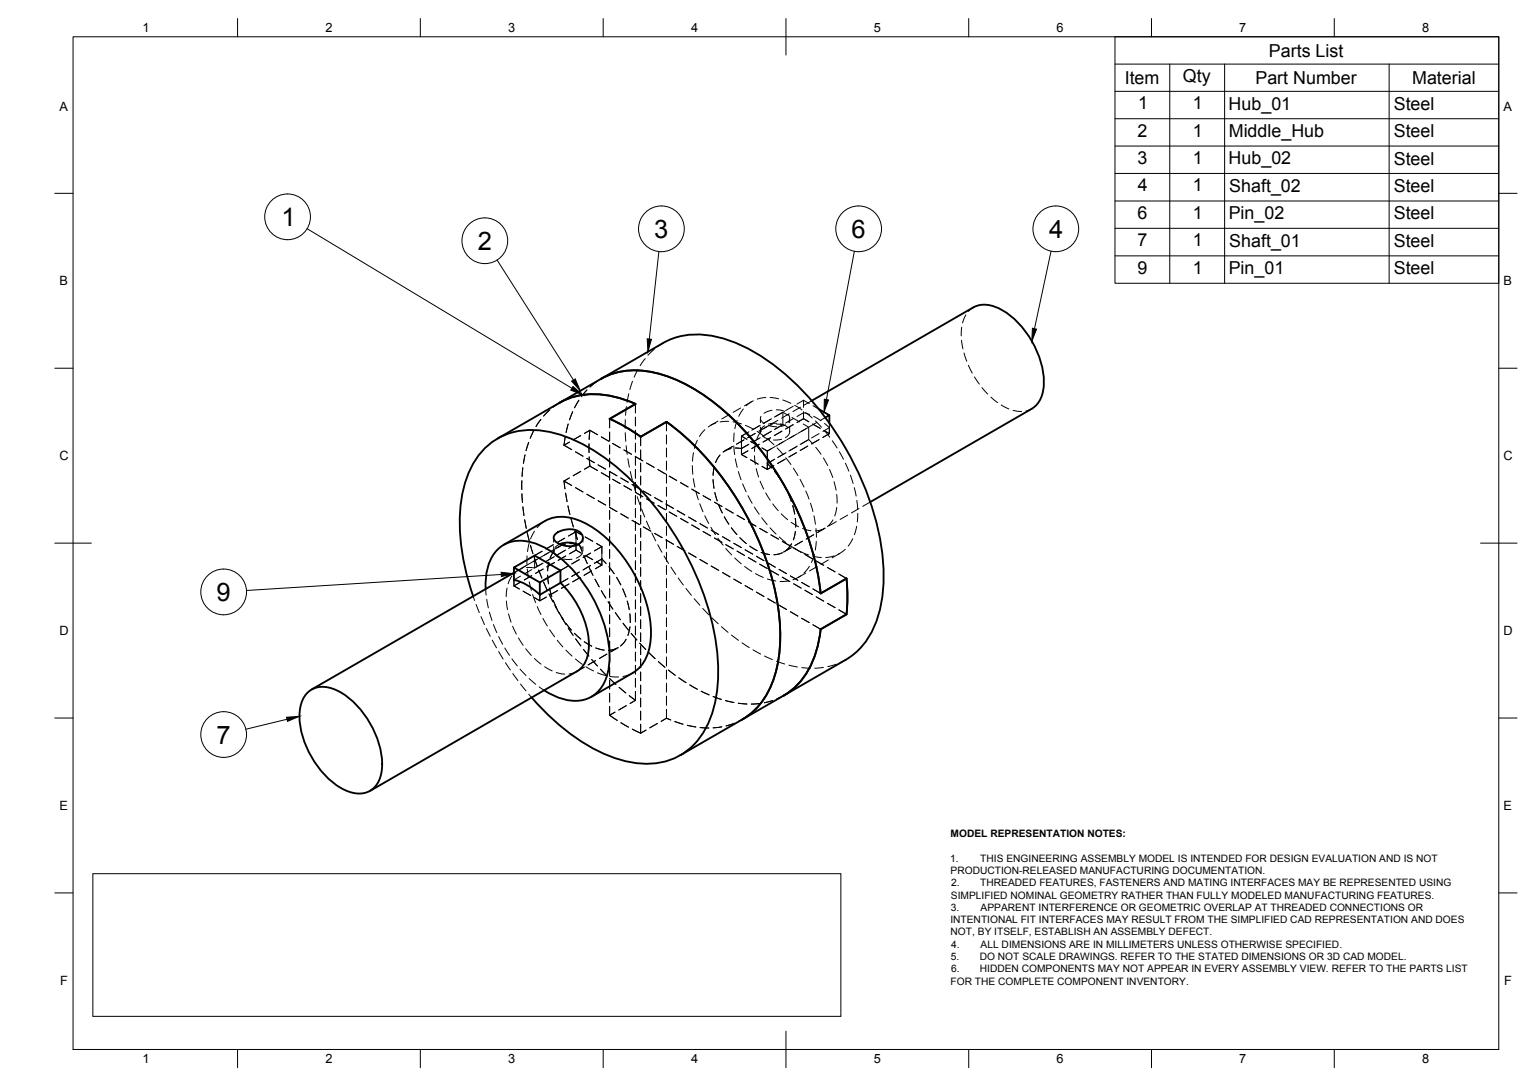
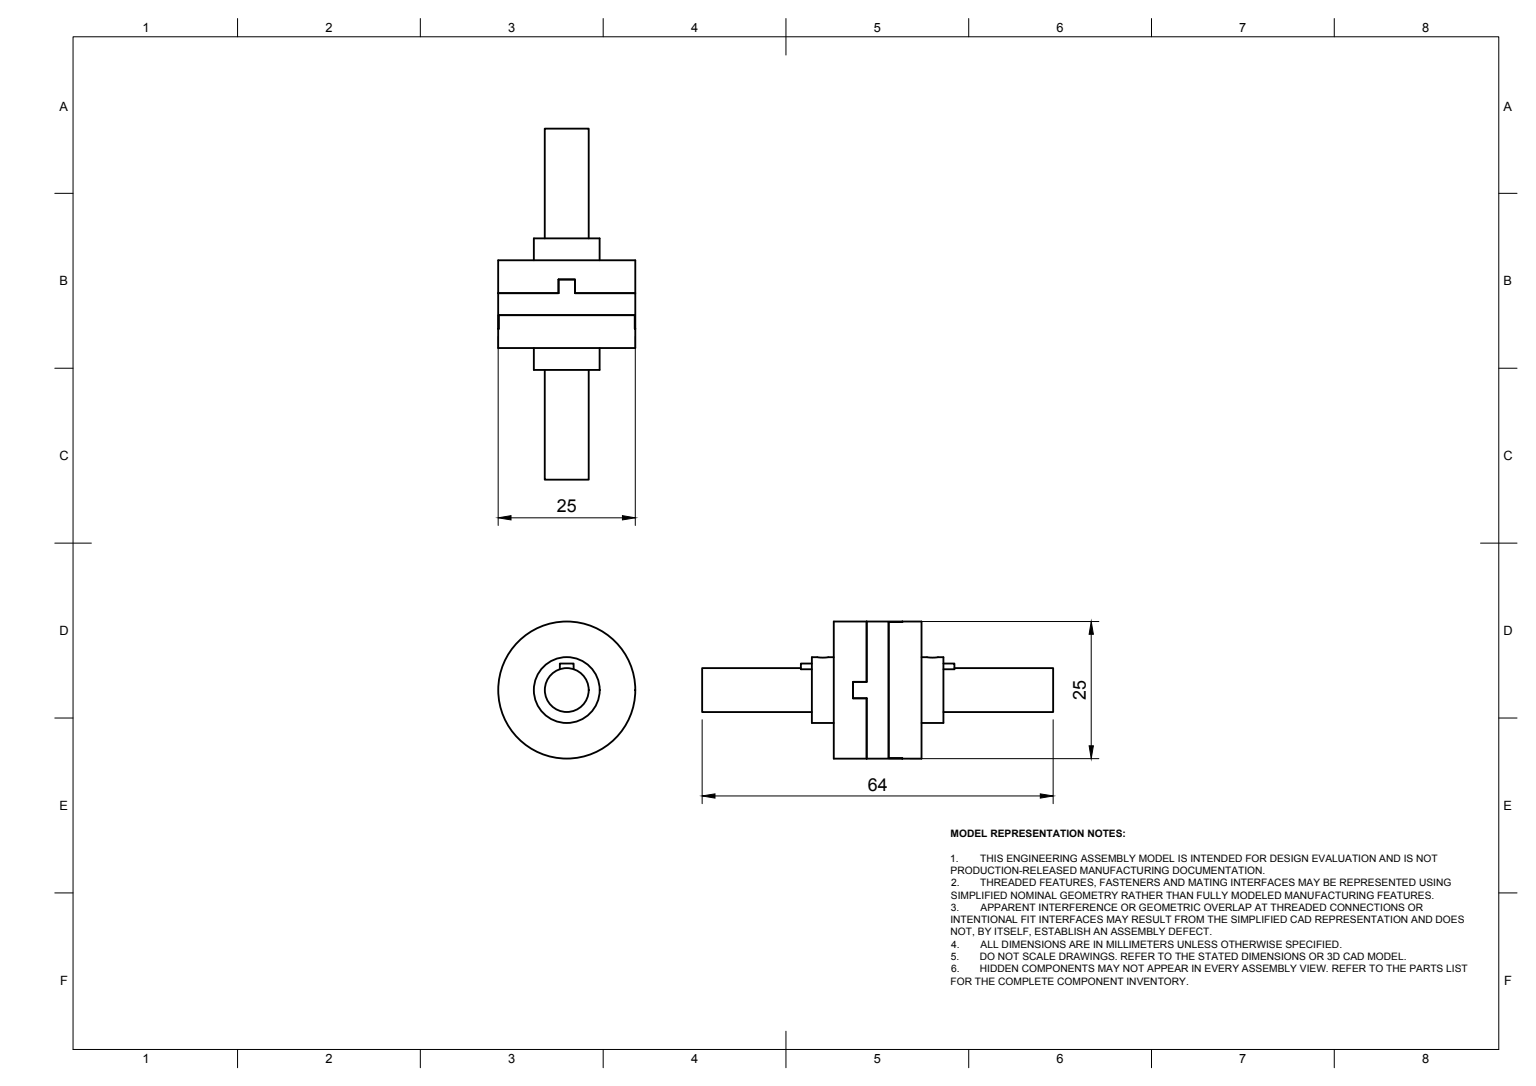
ISO-10303-21;
HEADER;
/* Generated by software containing ST-Developer
 * from STEP Tools, Inc. (www.steptools.com) 
 */

FILE_DESCRIPTION(
/* description */ (''),
/* implementation_level */ '2;1');

FILE_NAME(
/* name */ 'BR-256',
/* time_stamp */ '2026-10-05T22:24:12-07:00',
/* author */ (''),
/* organization */ (''),
/* preprocessor_version */ 'ST-DEVELOPER v20.2',
/* originating_system */ 'Autodesk Translation Framework v15.15.0.0',
/* authorisation */ '');

FILE_SCHEMA (('AUTOMOTIVE_DESIGN { 1 0 10303 214 3 1 1 }'));
ENDSEC;

DATA;
#10=MECHANICAL_DESIGN_GEOMETRIC_PRESENTATION_REPRESENTATION('',(#53,#54,
#55,#56,#57,#58,#59),#2116);
#11=ITEM_DEFINED_TRANSFORMATION($,$,#1233,#1347);
#12=ITEM_DEFINED_TRANSFORMATION($,$,#1260,#1348);
#13=ITEM_DEFINED_TRANSFORMATION($,$,#1282,#1349);
#14=ITEM_DEFINED_TRANSFORMATION($,$,#1309,#1350);
#15=ITEM_DEFINED_TRANSFORMATION($,$,#1321,#1351);
#16=ITEM_DEFINED_TRANSFORMATION($,$,#1328,#1352);
#17=ITEM_DEFINED_TRANSFORMATION($,$,#1340,#1353);
#18=(
REPRESENTATION_RELATIONSHIP($,$,#2145,#2144)
REPRESENTATION_RELATIONSHIP_WITH_TRANSFORMATION(#11)
SHAPE_REPRESENTATION_RELATIONSHIP()
);
#19=(
REPRESENTATION_RELATIONSHIP($,$,#2146,#2144)
REPRESENTATION_RELATIONSHIP_WITH_TRANSFORMATION(#12)
SHAPE_REPRESENTATION_RELATIONSHIP()
);
#20=(
REPRESENTATION_RELATIONSHIP($,$,#2147,#2144)
REPRESENTATION_RELATIONSHIP_WITH_TRANSFORMATION(#13)
SHAPE_REPRESENTATION_RELATIONSHIP()
);
#21=(
REPRESENTATION_RELATIONSHIP($,$,#2148,#2144)
REPRESENTATION_RELATIONSHIP_WITH_TRANSFORMATION(#14)
SHAPE_REPRESENTATION_RELATIONSHIP()
);
#22=(
REPRESENTATION_RELATIONSHIP($,$,#2149,#2144)
REPRESENTATION_RELATIONSHIP_WITH_TRANSFORMATION(#15)
SHAPE_REPRESENTATION_RELATIONSHIP()
);
#23=(
REPRESENTATION_RELATIONSHIP($,$,#2150,#2144)
REPRESENTATION_RELATIONSHIP_WITH_TRANSFORMATION(#16)
SHAPE_REPRESENTATION_RELATIONSHIP()
);
#24=(
REPRESENTATION_RELATIONSHIP($,$,#2151,#2144)
REPRESENTATION_RELATIONSHIP_WITH_TRANSFORMATION(#17)
SHAPE_REPRESENTATION_RELATIONSHIP()
);
#25=CONTEXT_DEPENDENT_SHAPE_REPRESENTATION(#18,#2137);
#26=CONTEXT_DEPENDENT_SHAPE_REPRESENTATION(#19,#2138);
#27=CONTEXT_DEPENDENT_SHAPE_REPRESENTATION(#20,#2139);
#28=CONTEXT_DEPENDENT_SHAPE_REPRESENTATION(#21,#2140);
#29=CONTEXT_DEPENDENT_SHAPE_REPRESENTATION(#22,#2141);
#30=CONTEXT_DEPENDENT_SHAPE_REPRESENTATION(#23,#2142);
#31=CONTEXT_DEPENDENT_SHAPE_REPRESENTATION(#24,#2143);
#32=NEXT_ASSEMBLY_USAGE_OCCURRENCE('Hub_01:1','Hub_01:1','Hub_01:1',#2153,
#2154,'Hub_01:1');
#33=NEXT_ASSEMBLY_USAGE_OCCURRENCE('Middle_Hub:1','Middle_Hub:1',
'Middle_Hub:1',#2153,#2155,'Middle_Hub:1');
#34=NEXT_ASSEMBLY_USAGE_OCCURRENCE('Hub_02:1','Hub_02:1','Hub_02:1',#2153,
#2156,'Hub_02:1');
#35=NEXT_ASSEMBLY_USAGE_OCCURRENCE('Shaft_02:1','Shaft_02:1',
'Shaft_02:1',#2153,#2157,'Shaft_02:1');
#36=NEXT_ASSEMBLY_USAGE_OCCURRENCE('Pin_02:1','Pin_02:1','Pin_02:1',#2153,
#2158,'Pin_02:1');
#37=NEXT_ASSEMBLY_USAGE_OCCURRENCE('Shaft_01:1','Shaft_01:1',
'Shaft_01:1',#2153,#2159,'Shaft_01:1');
#38=NEXT_ASSEMBLY_USAGE_OCCURRENCE('Pin_01:1','Pin_01:1','Pin_01:1',#2153,
#2160,'Pin_01:1');
#39=SHAPE_REPRESENTATION_RELATIONSHIP('SRR','None',#2145,#46);
#40=SHAPE_REPRESENTATION_RELATIONSHIP('SRR','None',#2146,#47);
#41=SHAPE_REPRESENTATION_RELATIONSHIP('SRR','None',#2147,#48);
#42=SHAPE_REPRESENTATION_RELATIONSHIP('SRR','None',#2148,#49);
#43=SHAPE_REPRESENTATION_RELATIONSHIP('SRR','None',#2149,#50);
#44=SHAPE_REPRESENTATION_RELATIONSHIP('SRR','None',#2150,#51);
#45=SHAPE_REPRESENTATION_RELATIONSHIP('SRR','None',#2151,#52);
#46=ADVANCED_BREP_SHAPE_REPRESENTATION('',(#60),#2109);
#47=ADVANCED_BREP_SHAPE_REPRESENTATION('',(#61),#2110);
#48=ADVANCED_BREP_SHAPE_REPRESENTATION('',(#62),#2111);
#49=ADVANCED_BREP_SHAPE_REPRESENTATION('',(#63),#2112);
#50=ADVANCED_BREP_SHAPE_REPRESENTATION('',(#64),#2113);
#51=ADVANCED_BREP_SHAPE_REPRESENTATION('',(#65),#2114);
#52=ADVANCED_BREP_SHAPE_REPRESENTATION('',(#66),#2115);
#53=STYLED_ITEM('',(#2189),#60);
#54=STYLED_ITEM('',(#2190),#61);
#55=STYLED_ITEM('',(#2191),#62);
#56=STYLED_ITEM('',(#2192),#63);
#57=STYLED_ITEM('',(#2192),#64);
#58=STYLED_ITEM('',(#2192),#65);
#59=STYLED_ITEM('',(#2192),#66);
#60=MANIFOLD_SOLID_BREP('Body1',#1147);
#61=MANIFOLD_SOLID_BREP('Body1',#1148);
#62=MANIFOLD_SOLID_BREP('Body1',#1149);
#63=MANIFOLD_SOLID_BREP('Body1',#1150);
#64=MANIFOLD_SOLID_BREP('Body1',#1151);
#65=MANIFOLD_SOLID_BREP('Body1',#1152);
#66=MANIFOLD_SOLID_BREP('Body1',#1153);
#67=FACE_BOUND('',#201,.T.);
#68=FACE_BOUND('',#211,.T.);
#69=FACE_BOUND('',#213,.T.);
#70=FACE_BOUND('',#215,.T.);
#71=FACE_BOUND('',#230,.T.);
#72=FACE_BOUND('',#234,.T.);
#73=FACE_BOUND('',#237,.T.);
#74=FACE_BOUND('',#239,.T.);
#75=PLANE('',#1236);
#76=PLANE('',#1237);
#77=PLANE('',#1238);
#78=PLANE('',#1239);
#79=PLANE('',#1243);
#80=PLANE('',#1244);
#81=PLANE('',#1245);
#82=PLANE('',#1248);
#83=PLANE('',#1250);
#84=PLANE('',#1256);
#85=PLANE('',#1257);
#86=PLANE('',#1261);
#87=PLANE('',#1262);
#88=PLANE('',#1263);
#89=PLANE('',#1267);
#90=PLANE('',#1269);
#91=PLANE('',#1271);
#92=PLANE('',#1272);
#93=PLANE('',#1273);
#94=PLANE('',#1276);
#95=PLANE('',#1278);
#96=PLANE('',#1285);
#97=PLANE('',#1286);
#98=PLANE('',#1287);
#99=PLANE('',#1288);
#100=PLANE('',#1295);
#101=PLANE('',#1297);
#102=PLANE('',#1298);
#103=PLANE('',#1299);
#104=PLANE('',#1303);
#105=PLANE('',#1305);
#106=PLANE('',#1308);
#107=PLANE('',#1310);
#108=PLANE('',#1311);
#109=PLANE('',#1312);
#110=PLANE('',#1313);
#111=PLANE('',#1315);
#112=PLANE('',#1320);
#113=PLANE('',#1322);
#114=PLANE('',#1323);
#115=PLANE('',#1324);
#116=PLANE('',#1325);
#117=PLANE('',#1326);
#118=PLANE('',#1327);
#119=PLANE('',#1329);
#120=PLANE('',#1330);
#121=PLANE('',#1332);
#122=PLANE('',#1333);
#123=PLANE('',#1338);
#124=PLANE('',#1339);
#125=PLANE('',#1341);
#126=PLANE('',#1342);
#127=PLANE('',#1343);
#128=PLANE('',#1344);
#129=PLANE('',#1345);
#130=PLANE('',#1346);
#131=FACE_OUTER_BOUND('',#198,.T.);
#132=FACE_OUTER_BOUND('',#199,.T.);
#133=FACE_OUTER_BOUND('',#200,.T.);
#134=FACE_OUTER_BOUND('',#202,.T.);
#135=FACE_OUTER_BOUND('',#203,.T.);
#136=FACE_OUTER_BOUND('',#204,.T.);
#137=FACE_OUTER_BOUND('',#205,.T.);
#138=FACE_OUTER_BOUND('',#206,.T.);
#139=FACE_OUTER_BOUND('',#207,.T.);
#140=FACE_OUTER_BOUND('',#208,.T.);
#141=FACE_OUTER_BOUND('',#209,.T.);
#142=FACE_OUTER_BOUND('',#210,.T.);
#143=FACE_OUTER_BOUND('',#212,.T.);
#144=FACE_OUTER_BOUND('',#214,.T.);
#145=FACE_OUTER_BOUND('',#216,.T.);
#146=FACE_OUTER_BOUND('',#217,.T.);
#147=FACE_OUTER_BOUND('',#218,.T.);
#148=FACE_OUTER_BOUND('',#219,.T.);
#149=FACE_OUTER_BOUND('',#220,.T.);
#150=FACE_OUTER_BOUND('',#221,.T.);
#151=FACE_OUTER_BOUND('',#222,.T.);
#152=FACE_OUTER_BOUND('',#223,.T.);
#153=FACE_OUTER_BOUND('',#224,.T.);
#154=FACE_OUTER_BOUND('',#225,.T.);
#155=FACE_OUTER_BOUND('',#226,.T.);
#156=FACE_OUTER_BOUND('',#227,.T.);
#157=FACE_OUTER_BOUND('',#228,.T.);
#158=FACE_OUTER_BOUND('',#229,.T.);
#159=FACE_OUTER_BOUND('',#231,.T.);
#160=FACE_OUTER_BOUND('',#232,.T.);
#161=FACE_OUTER_BOUND('',#233,.T.);
#162=FACE_OUTER_BOUND('',#235,.T.);
#163=FACE_OUTER_BOUND('',#236,.T.);
#164=FACE_OUTER_BOUND('',#238,.T.);
#165=FACE_OUTER_BOUND('',#240,.T.);
#166=FACE_OUTER_BOUND('',#241,.T.);
#167=FACE_OUTER_BOUND('',#242,.T.);
#168=FACE_OUTER_BOUND('',#243,.T.);
#169=FACE_OUTER_BOUND('',#244,.T.);
#170=FACE_OUTER_BOUND('',#245,.T.);
#171=FACE_OUTER_BOUND('',#246,.T.);
#172=FACE_OUTER_BOUND('',#247,.T.);
#173=FACE_OUTER_BOUND('',#248,.T.);
#174=FACE_OUTER_BOUND('',#249,.T.);
#175=FACE_OUTER_BOUND('',#250,.T.);
#176=FACE_OUTER_BOUND('',#251,.T.);
#177=FACE_OUTER_BOUND('',#252,.T.);
#178=FACE_OUTER_BOUND('',#253,.T.);
#179=FACE_OUTER_BOUND('',#254,.T.);
#180=FACE_OUTER_BOUND('',#255,.T.);
#181=FACE_OUTER_BOUND('',#256,.T.);
#182=FACE_OUTER_BOUND('',#257,.T.);
#183=FACE_OUTER_BOUND('',#258,.T.);
#184=FACE_OUTER_BOUND('',#259,.T.);
#185=FACE_OUTER_BOUND('',#260,.T.);
#186=FACE_OUTER_BOUND('',#261,.T.);
#187=FACE_OUTER_BOUND('',#262,.T.);
#188=FACE_OUTER_BOUND('',#263,.T.);
#189=FACE_OUTER_BOUND('',#264,.T.);
#190=FACE_OUTER_BOUND('',#265,.T.);
#191=FACE_OUTER_BOUND('',#266,.T.);
#192=FACE_OUTER_BOUND('',#267,.T.);
#193=FACE_OUTER_BOUND('',#268,.T.);
#194=FACE_OUTER_BOUND('',#269,.T.);
#195=FACE_OUTER_BOUND('',#270,.T.);
#196=FACE_OUTER_BOUND('',#271,.T.);
#197=FACE_OUTER_BOUND('',#272,.T.);
#198=EDGE_LOOP('',(#773,#774,#775,#776));
#199=EDGE_LOOP('',(#777,#778,#779,#780));
#200=EDGE_LOOP('',(#781,#782,#783,#784));
#201=EDGE_LOOP('',(#785));
#202=EDGE_LOOP('',(#786,#787,#788,#789));
#203=EDGE_LOOP('',(#790,#791,#792,#793));
#204=EDGE_LOOP('',(#794,#795,#796,#797));
#205=EDGE_LOOP('',(#798,#799,#800,#801));
#206=EDGE_LOOP('',(#802,#803,#804,#805));
#207=EDGE_LOOP('',(#806,#807,#808,#809));
#208=EDGE_LOOP('',(#810,#811));
#209=EDGE_LOOP('',(#812,#813,#814));
#210=EDGE_LOOP('',(#815,#816,#817,#818));
#211=EDGE_LOOP('',(#819));
#212=EDGE_LOOP('',(#820));
#213=EDGE_LOOP('',(#821,#822,#823,#824));
#214=EDGE_LOOP('',(#825));
#215=EDGE_LOOP('',(#826));
#216=EDGE_LOOP('',(#827,#828,#829,#830,#831,#832,#833,#834,#835,#836,#837,
#838));
#217=EDGE_LOOP('',(#839,#840,#841,#842));
#218=EDGE_LOOP('',(#843,#844,#845,#846));
#219=EDGE_LOOP('',(#847,#848,#849,#850,#851));
#220=EDGE_LOOP('',(#852,#853));
#221=EDGE_LOOP('',(#854,#855));
#222=EDGE_LOOP('',(#856,#857,#858,#859));
#223=EDGE_LOOP('',(#860,#861,#862,#863));
#224=EDGE_LOOP('',(#864,#865,#866,#867));
#225=EDGE_LOOP('',(#868,#869));
#226=EDGE_LOOP('',(#870,#871,#872));
#227=EDGE_LOOP('',(#873,#874,#875,#876,#877,#878,#879,#880,#881,#882,#883,
#884,#885,#886,#887,#888,#889,#890,#891,#892));
#228=EDGE_LOOP('',(#893,#894,#895,#896,#897));
#229=EDGE_LOOP('',(#898,#899,#900,#901));
#230=EDGE_LOOP('',(#902));
#231=EDGE_LOOP('',(#903,#904,#905,#906));
#232=EDGE_LOOP('',(#907,#908,#909,#910));
#233=EDGE_LOOP('',(#911));
#234=EDGE_LOOP('',(#912,#913,#914,#915));
#235=EDGE_LOOP('',(#916,#917,#918,#919));
#236=EDGE_LOOP('',(#920,#921,#922,#923));
#237=EDGE_LOOP('',(#924,#925));
#238=EDGE_LOOP('',(#926));
#239=EDGE_LOOP('',(#927));
#240=EDGE_LOOP('',(#928,#929,#930,#931));
#241=EDGE_LOOP('',(#932,#933,#934,#935));
#242=EDGE_LOOP('',(#936,#937,#938,#939,#940));
#243=EDGE_LOOP('',(#941,#942));
#244=EDGE_LOOP('',(#943,#944));
#245=EDGE_LOOP('',(#945,#946,#947,#948,#949,#950,#951,#952,#953,#954,#955,
#956));
#246=EDGE_LOOP('',(#957,#958,#959,#960));
#247=EDGE_LOOP('',(#961,#962,#963,#964));
#248=EDGE_LOOP('',(#965,#966,#967,#968));
#249=EDGE_LOOP('',(#969,#970,#971,#972));
#250=EDGE_LOOP('',(#973,#974,#975,#976));
#251=EDGE_LOOP('',(#977,#978,#979,#980,#981));
#252=EDGE_LOOP('',(#982,#983,#984,#985,#986,#987,#988,#989));
#253=EDGE_LOOP('',(#990));
#254=EDGE_LOOP('',(#991,#992,#993,#994));
#255=EDGE_LOOP('',(#995,#996,#997,#998));
#256=EDGE_LOOP('',(#999,#1000,#1001,#1002));
#257=EDGE_LOOP('',(#1003,#1004,#1005,#1006));
#258=EDGE_LOOP('',(#1007,#1008,#1009,#1010));
#259=EDGE_LOOP('',(#1011,#1012,#1013,#1014));
#260=EDGE_LOOP('',(#1015,#1016,#1017,#1018));
#261=EDGE_LOOP('',(#1019,#1020,#1021,#1022));
#262=EDGE_LOOP('',(#1023,#1024,#1025,#1026));
#263=EDGE_LOOP('',(#1027,#1028,#1029,#1030));
#264=EDGE_LOOP('',(#1031,#1032,#1033,#1034,#1035,#1036,#1037,#1038));
#265=EDGE_LOOP('',(#1039));
#266=EDGE_LOOP('',(#1040,#1041,#1042,#1043,#1044));
#267=EDGE_LOOP('',(#1045,#1046,#1047,#1048));
#268=EDGE_LOOP('',(#1049,#1050,#1051,#1052));
#269=EDGE_LOOP('',(#1053,#1054,#1055,#1056));
#270=EDGE_LOOP('',(#1057,#1058,#1059,#1060));
#271=EDGE_LOOP('',(#1061,#1062,#1063,#1064));
#272=EDGE_LOOP('',(#1065,#1066,#1067,#1068));
#273=B_SPLINE_CURVE_WITH_KNOTS('',3,(#1710,#1711,#1712,#1713,#1714,#1715,
#1716,#1717,#1718,#1719,#1720,#1721,#1722,#1723,#1724,#1725,#1726,#1727,
#1728,#1729,#1730,#1731,#1732,#1733,#1734,#1735,#1736,#1737,#1738,#1739,
#1740,#1741,#1742,#1743),.UNSPECIFIED.,.T.,.F.,(4,2,2,2,2,2,2,2,2,2,2,2,
2,2,2,2,4),(0.,0.0377449625945589,0.0754899251891177,0.113233879657539,
0.150977834125959,0.18872178859438,0.226465743062801,0.26421070565736,0.301955668251919,
0.339700630846477,0.377445593441036,0.415189547909457,0.452933502377878,
0.490677456846299,0.52842141131472,0.566166373909278,0.603911336503837),
 .UNSPECIFIED.);
#274=B_SPLINE_CURVE_WITH_KNOTS('',3,(#1872,#1873,#1874,#1875,#1876,#1877,
#1878,#1879,#1880,#1881,#1882,#1883,#1884,#1885,#1886,#1887,#1888,#1889),
 .UNSPECIFIED.,.F.,.F.,(4,2,2,2,2,2,2,2,4),(0.,0.0377449625945587,0.0754899251891175,
0.113233879657538,0.150977834125959,0.18872178859438,0.226465743062801,
0.264210705657359,0.301955668251918),.UNSPECIFIED.);
#275=B_SPLINE_CURVE_WITH_KNOTS('',3,(#1890,#1891,#1892,#1893,#1894,#1895,
#1896,#1897,#1898,#1899,#1900,#1901,#1902,#1903,#1904,#1905,#1906,#1907),
 .UNSPECIFIED.,.F.,.F.,(4,2,2,2,2,2,2,2,4),(0.301955668251918,0.339700630846477,
0.377445593441036,0.415189547909457,0.452933502377877,0.490677456846298,
0.528421411314719,0.566166373909278,0.603911336503836),.UNSPECIFIED.);
#276=LINE('',#1709,#381);
#277=LINE('',#1747,#382);
#278=LINE('',#1749,#383);
#279=LINE('',#1751,#384);
#280=LINE('',#1752,#385);
#281=LINE('',#1755,#386);
#282=LINE('',#1757,#387);
#283=LINE('',#1758,#388);
#284=LINE('',#1761,#389);
#285=LINE('',#1763,#390);
#286=LINE('',#1764,#391);
#287=LINE('',#1772,#392);
#288=LINE('',#1774,#393);
#289=LINE('',#1776,#394);
#290=LINE('',#1777,#395);
#291=LINE('',#1781,#396);
#292=LINE('',#1783,#397);
#293=LINE('',#1785,#398);
#294=LINE('',#1786,#399);
#295=LINE('',#1800,#400);
#296=LINE('',#1807,#401);
#297=LINE('',#1812,#402);
#298=LINE('',#1814,#403);
#299=LINE('',#1816,#404);
#300=LINE('',#1817,#405);
#301=LINE('',#1821,#406);
#302=LINE('',#1823,#407);
#303=LINE('',#1825,#408);
#304=LINE('',#1826,#409);
#305=LINE('',#1839,#410);
#306=LINE('',#1841,#411);
#307=LINE('',#1843,#412);
#308=LINE('',#1844,#413);
#309=LINE('',#1848,#414);
#310=LINE('',#1850,#415);
#311=LINE('',#1852,#416);
#312=LINE('',#1853,#417);
#313=LINE('',#1864,#418);
#314=LINE('',#1870,#419);
#315=LINE('',#1911,#420);
#316=LINE('',#1913,#421);
#317=LINE('',#1915,#422);
#318=LINE('',#1916,#423);
#319=LINE('',#1919,#424);
#320=LINE('',#1921,#425);
#321=LINE('',#1922,#426);
#322=LINE('',#1925,#427);
#323=LINE('',#1927,#428);
#324=LINE('',#1928,#429);
#325=LINE('',#1937,#430);
#326=LINE('',#1945,#431);
#327=LINE('',#1947,#432);
#328=LINE('',#1949,#433);
#329=LINE('',#1950,#434);
#330=LINE('',#1954,#435);
#331=LINE('',#1956,#436);
#332=LINE('',#1958,#437);
#333=LINE('',#1959,#438);
#334=LINE('',#1970,#439);
#335=LINE('',#1976,#440);
#336=LINE('',#1978,#441);
#337=LINE('',#1980,#442);
#338=LINE('',#1981,#443);
#339=LINE('',#1984,#444);
#340=LINE('',#1986,#445);
#341=LINE('',#1987,#446);
#342=LINE('',#1991,#447);
#343=LINE('',#1992,#448);
#344=LINE('',#1993,#449);
#345=LINE('',#2002,#450);
#346=LINE('',#2009,#451);
#347=LINE('',#2011,#452);
#348=LINE('',#2013,#453);
#349=LINE('',#2014,#454);
#350=LINE('',#2017,#455);
#351=LINE('',#2019,#456);
#352=LINE('',#2020,#457);
#353=LINE('',#2023,#458);
#354=LINE('',#2025,#459);
#355=LINE('',#2026,#460);
#356=LINE('',#2028,#461);
#357=LINE('',#2029,#462);
#358=LINE('',#2036,#463);
#359=LINE('',#2038,#464);
#360=LINE('',#2040,#465);
#361=LINE('',#2041,#466);
#362=LINE('',#2046,#467);
#363=LINE('',#2047,#468);
#364=LINE('',#2050,#469);
#365=LINE('',#2051,#470);
#366=LINE('',#2054,#471);
#367=LINE('',#2055,#472);
#368=LINE('',#2060,#473);
#369=LINE('',#2069,#474);
#370=LINE('',#2071,#475);
#371=LINE('',#2073,#476);
#372=LINE('',#2074,#477);
#373=LINE('',#2077,#478);
#374=LINE('',#2079,#479);
#375=LINE('',#2080,#480);
#376=LINE('',#2083,#481);
#377=LINE('',#2085,#482);
#378=LINE('',#2086,#483);
#379=LINE('',#2088,#484);
#380=LINE('',#2089,#485);
#381=VECTOR('',#1362,1.);
#382=VECTOR('',#1365,10.);
#383=VECTOR('',#1366,10.);
#384=VECTOR('',#1367,10.);
#385=VECTOR('',#1368,10.);
#386=VECTOR('',#1371,10.);
#387=VECTOR('',#1372,10.);
#388=VECTOR('',#1373,10.);
#389=VECTOR('',#1376,10.);
#390=VECTOR('',#1377,10.);
#391=VECTOR('',#1378,10.);
#392=VECTOR('',#1389,10.);
#393=VECTOR('',#1390,10.);
#394=VECTOR('',#1391,10.);
#395=VECTOR('',#1392,10.);
#396=VECTOR('',#1395,10.);
#397=VECTOR('',#1396,10.);
#398=VECTOR('',#1397,10.);
#399=VECTOR('',#1398,10.);
#400=VECTOR('',#1419,6.);
#401=VECTOR('',#1430,12.5);
#402=VECTOR('',#1435,10.);
#403=VECTOR('',#1436,10.);
#404=VECTOR('',#1437,10.);
#405=VECTOR('',#1438,10.);
#406=VECTOR('',#1441,10.);
#407=VECTOR('',#1442,10.);
#408=VECTOR('',#1443,10.);
#409=VECTOR('',#1444,10.);
#410=VECTOR('',#1463,10.);
#411=VECTOR('',#1464,10.);
#412=VECTOR('',#1465,10.);
#413=VECTOR('',#1466,10.);
#414=VECTOR('',#1469,10.);
#415=VECTOR('',#1470,10.);
#416=VECTOR('',#1471,10.);
#417=VECTOR('',#1472,10.);
#418=VECTOR('',#1491,12.5);
#419=VECTOR('',#1498,0.999999999999999);
#420=VECTOR('',#1501,10.);
#421=VECTOR('',#1502,10.);
#422=VECTOR('',#1503,10.);
#423=VECTOR('',#1504,10.);
#424=VECTOR('',#1507,10.);
#425=VECTOR('',#1508,10.);
#426=VECTOR('',#1509,10.);
#427=VECTOR('',#1512,10.);
#428=VECTOR('',#1513,10.);
#429=VECTOR('',#1514,10.);
#430=VECTOR('',#1527,6.);
#431=VECTOR('',#1536,10.);
#432=VECTOR('',#1537,10.);
#433=VECTOR('',#1538,10.);
#434=VECTOR('',#1539,10.);
#435=VECTOR('',#1542,10.);
#436=VECTOR('',#1543,10.);
#437=VECTOR('',#1544,10.);
#438=VECTOR('',#1545,10.);
#439=VECTOR('',#1564,12.5);
#440=VECTOR('',#1571,10.);
#441=VECTOR('',#1572,10.);
#442=VECTOR('',#1573,10.);
#443=VECTOR('',#1574,10.);
#444=VECTOR('',#1577,10.);
#445=VECTOR('',#1578,10.);
#446=VECTOR('',#1579,10.);
#447=VECTOR('',#1582,10.);
#448=VECTOR('',#1583,10.);
#449=VECTOR('',#1584,10.);
#450=VECTOR('',#1597,4.);
#451=VECTOR('',#1606,10.);
#452=VECTOR('',#1607,10.);
#453=VECTOR('',#1608,10.);
#454=VECTOR('',#1609,10.);
#455=VECTOR('',#1612,10.);
#456=VECTOR('',#1613,10.);
#457=VECTOR('',#1614,10.);
#458=VECTOR('',#1617,10.);
#459=VECTOR('',#1618,10.);
#460=VECTOR('',#1619,10.);
#461=VECTOR('',#1622,10.);
#462=VECTOR('',#1623,10.);
#463=VECTOR('',#1632,10.);
#464=VECTOR('',#1633,10.);
#465=VECTOR('',#1634,10.);
#466=VECTOR('',#1635,10.);
#467=VECTOR('',#1640,10.);
#468=VECTOR('',#1641,10.);
#469=VECTOR('',#1644,10.);
#470=VECTOR('',#1645,10.);
#471=VECTOR('',#1648,10.);
#472=VECTOR('',#1649,10.);
#473=VECTOR('',#1654,4.);
#474=VECTOR('',#1667,10.);
#475=VECTOR('',#1668,10.);
#476=VECTOR('',#1669,10.);
#477=VECTOR('',#1670,10.);
#478=VECTOR('',#1673,10.);
#479=VECTOR('',#1674,10.);
#480=VECTOR('',#1675,10.);
#481=VECTOR('',#1678,10.);
#482=VECTOR('',#1679,10.);
#483=VECTOR('',#1680,10.);
#484=VECTOR('',#1683,10.);
#485=VECTOR('',#1684,10.);
#486=CIRCLE('',#1235,1.);
#487=CIRCLE('',#1240,4.);
#488=CIRCLE('',#1242,4.);
#489=CIRCLE('',#1246,12.5);
#490=CIRCLE('',#1247,12.5);
#491=CIRCLE('',#1249,12.5);
#492=CIRCLE('',#1251,12.5);
#493=CIRCLE('',#1252,12.5);
#494=CIRCLE('',#1254,6.);
#495=CIRCLE('',#1255,6.);
#496=CIRCLE('',#1258,12.5);
#497=CIRCLE('',#1264,12.5);
#498=CIRCLE('',#1265,12.5);
#499=CIRCLE('',#1266,12.5);
#500=CIRCLE('',#1268,12.5);
#501=CIRCLE('',#1270,12.5);
#502=CIRCLE('',#1274,12.5);
#503=CIRCLE('',#1275,12.5);
#504=CIRCLE('',#1277,12.5);
#505=CIRCLE('',#1279,12.5);
#506=CIRCLE('',#1280,12.5);
#507=CIRCLE('',#1284,0.999999999999999);
#508=CIRCLE('',#1289,6.);
#509=CIRCLE('',#1290,4.);
#510=CIRCLE('',#1292,4.);
#511=CIRCLE('',#1294,6.);
#512=CIRCLE('',#1296,12.5);
#513=CIRCLE('',#1300,12.5);
#514=CIRCLE('',#1301,12.5);
#515=CIRCLE('',#1302,12.5);
#516=CIRCLE('',#1304,12.5);
#517=CIRCLE('',#1306,12.5);
#518=CIRCLE('',#1314,4.);
#519=CIRCLE('',#1316,4.);
#520=CIRCLE('',#1317,4.);
#521=CIRCLE('',#1319,4.);
#522=CIRCLE('',#1331,4.);
#523=CIRCLE('',#1335,4.);
#524=CIRCLE('',#1336,4.);
#525=CIRCLE('',#1337,4.);
#526=VERTEX_POINT('',#1706);
#527=VERTEX_POINT('',#1708);
#528=VERTEX_POINT('',#1745);
#529=VERTEX_POINT('',#1746);
#530=VERTEX_POINT('',#1748);
#531=VERTEX_POINT('',#1750);
#532=VERTEX_POINT('',#1754);
#533=VERTEX_POINT('',#1756);
#534=VERTEX_POINT('',#1760);
#535=VERTEX_POINT('',#1762);
#536=VERTEX_POINT('',#1770);
#537=VERTEX_POINT('',#1771);
#538=VERTEX_POINT('',#1773);
#539=VERTEX_POINT('',#1775);
#540=VERTEX_POINT('',#1779);
#541=VERTEX_POINT('',#1780);
#542=VERTEX_POINT('',#1782);
#543=VERTEX_POINT('',#1784);
#544=VERTEX_POINT('',#1793);
#545=VERTEX_POINT('',#1797);
#546=VERTEX_POINT('',#1799);
#547=VERTEX_POINT('',#1804);
#548=VERTEX_POINT('',#1810);
#549=VERTEX_POINT('',#1811);
#550=VERTEX_POINT('',#1813);
#551=VERTEX_POINT('',#1815);
#552=VERTEX_POINT('',#1819);
#553=VERTEX_POINT('',#1820);
#554=VERTEX_POINT('',#1822);
#555=VERTEX_POINT('',#1824);
#556=VERTEX_POINT('',#1829);
#557=VERTEX_POINT('',#1837);
#558=VERTEX_POINT('',#1838);
#559=VERTEX_POINT('',#1840);
#560=VERTEX_POINT('',#1842);
#561=VERTEX_POINT('',#1846);
#562=VERTEX_POINT('',#1847);
#563=VERTEX_POINT('',#1849);
#564=VERTEX_POINT('',#1851);
#565=VERTEX_POINT('',#1860);
#566=VERTEX_POINT('',#1867);
#567=VERTEX_POINT('',#1869);
#568=VERTEX_POINT('',#1871);
#569=VERTEX_POINT('',#1909);
#570=VERTEX_POINT('',#1910);
#571=VERTEX_POINT('',#1912);
#572=VERTEX_POINT('',#1914);
#573=VERTEX_POINT('',#1918);
#574=VERTEX_POINT('',#1920);
#575=VERTEX_POINT('',#1924);
#576=VERTEX_POINT('',#1926);
#577=VERTEX_POINT('',#1930);
#578=VERTEX_POINT('',#1936);
#579=VERTEX_POINT('',#1940);
#580=VERTEX_POINT('',#1943);
#581=VERTEX_POINT('',#1944);
#582=VERTEX_POINT('',#1946);
#583=VERTEX_POINT('',#1948);
#584=VERTEX_POINT('',#1952);
#585=VERTEX_POINT('',#1953);
#586=VERTEX_POINT('',#1955);
#587=VERTEX_POINT('',#1957);
#588=VERTEX_POINT('',#1962);
#589=VERTEX_POINT('',#1974);
#590=VERTEX_POINT('',#1975);
#591=VERTEX_POINT('',#1977);
#592=VERTEX_POINT('',#1979);
#593=VERTEX_POINT('',#1983);
#594=VERTEX_POINT('',#1985);
#595=VERTEX_POINT('',#1989);
#596=VERTEX_POINT('',#1990);
#597=VERTEX_POINT('',#1997);
#598=VERTEX_POINT('',#2001);
#599=VERTEX_POINT('',#2007);
#600=VERTEX_POINT('',#2008);
#601=VERTEX_POINT('',#2010);
#602=VERTEX_POINT('',#2012);
#603=VERTEX_POINT('',#2016);
#604=VERTEX_POINT('',#2018);
#605=VERTEX_POINT('',#2022);
#606=VERTEX_POINT('',#2024);
#607=VERTEX_POINT('',#2034);
#608=VERTEX_POINT('',#2035);
#609=VERTEX_POINT('',#2037);
#610=VERTEX_POINT('',#2039);
#611=VERTEX_POINT('',#2043);
#612=VERTEX_POINT('',#2045);
#613=VERTEX_POINT('',#2049);
#614=VERTEX_POINT('',#2053);
#615=VERTEX_POINT('',#2057);
#616=VERTEX_POINT('',#2059);
#617=VERTEX_POINT('',#2067);
#618=VERTEX_POINT('',#2068);
#619=VERTEX_POINT('',#2070);
#620=VERTEX_POINT('',#2072);
#621=VERTEX_POINT('',#2076);
#622=VERTEX_POINT('',#2078);
#623=VERTEX_POINT('',#2082);
#624=VERTEX_POINT('',#2084);
#625=EDGE_CURVE('',#526,#526,#486,.T.);
#626=EDGE_CURVE('',#526,#527,#276,.T.);
#627=EDGE_CURVE('',#527,#527,#273,.T.);
#628=EDGE_CURVE('',#528,#529,#277,.T.);
#629=EDGE_CURVE('',#530,#528,#278,.T.);
#630=EDGE_CURVE('',#530,#531,#279,.T.);
#631=EDGE_CURVE('',#529,#531,#280,.T.);
#632=EDGE_CURVE('',#532,#528,#281,.T.);
#633=EDGE_CURVE('',#533,#532,#282,.T.);
#634=EDGE_CURVE('',#533,#530,#283,.T.);
#635=EDGE_CURVE('',#534,#532,#284,.T.);
#636=EDGE_CURVE('',#535,#534,#285,.T.);
#637=EDGE_CURVE('',#533,#535,#286,.T.);
#638=EDGE_CURVE('',#535,#531,#487,.T.);
#639=EDGE_CURVE('',#529,#534,#488,.T.);
#640=EDGE_CURVE('',#536,#537,#287,.T.);
#641=EDGE_CURVE('',#538,#536,#288,.T.);
#642=EDGE_CURVE('',#538,#539,#289,.T.);
#643=EDGE_CURVE('',#537,#539,#290,.T.);
#644=EDGE_CURVE('',#540,#541,#291,.T.);
#645=EDGE_CURVE('',#542,#540,#292,.T.);
#646=EDGE_CURVE('',#542,#543,#293,.T.);
#647=EDGE_CURVE('',#541,#543,#294,.T.);
#648=EDGE_CURVE('',#539,#542,#489,.T.);
#649=EDGE_CURVE('',#543,#538,#490,.T.);
#650=EDGE_CURVE('',#541,#540,#491,.T.);
#651=EDGE_CURVE('',#537,#544,#492,.T.);
#652=EDGE_CURVE('',#544,#536,#493,.T.);
#653=EDGE_CURVE('',#545,#545,#494,.T.);
#654=EDGE_CURVE('',#545,#546,#295,.T.);
#655=EDGE_CURVE('',#546,#546,#495,.T.);
#656=EDGE_CURVE('',#547,#547,#496,.T.);
#657=EDGE_CURVE('',#547,#544,#296,.T.);
#658=EDGE_CURVE('',#548,#549,#297,.T.);
#659=EDGE_CURVE('',#548,#550,#298,.T.);
#660=EDGE_CURVE('',#551,#550,#299,.T.);
#661=EDGE_CURVE('',#549,#551,#300,.T.);
#662=EDGE_CURVE('',#552,#553,#301,.T.);
#663=EDGE_CURVE('',#552,#554,#302,.T.);
#664=EDGE_CURVE('',#555,#554,#303,.T.);
#665=EDGE_CURVE('',#553,#555,#304,.T.);
#666=EDGE_CURVE('',#550,#555,#497,.T.);
#667=EDGE_CURVE('',#554,#556,#498,.T.);
#668=EDGE_CURVE('',#556,#551,#499,.T.);
#669=EDGE_CURVE('',#549,#548,#500,.T.);
#670=EDGE_CURVE('',#553,#552,#501,.T.);
#671=EDGE_CURVE('',#557,#558,#305,.T.);
#672=EDGE_CURVE('',#557,#559,#306,.T.);
#673=EDGE_CURVE('',#560,#559,#307,.T.);
#674=EDGE_CURVE('',#558,#560,#308,.T.);
#675=EDGE_CURVE('',#561,#562,#309,.T.);
#676=EDGE_CURVE('',#561,#563,#310,.T.);
#677=EDGE_CURVE('',#564,#563,#311,.T.);
#678=EDGE_CURVE('',#562,#564,#312,.T.);
#679=EDGE_CURVE('',#559,#564,#502,.T.);
#680=EDGE_CURVE('',#563,#560,#503,.T.);
#681=EDGE_CURVE('',#557,#558,#504,.T.);
#682=EDGE_CURVE('',#565,#562,#505,.T.);
#683=EDGE_CURVE('',#561,#565,#506,.T.);
#684=EDGE_CURVE('',#556,#565,#313,.T.);
#685=EDGE_CURVE('',#566,#566,#507,.T.);
#686=EDGE_CURVE('',#566,#567,#314,.T.);
#687=EDGE_CURVE('',#568,#567,#274,.T.);
#688=EDGE_CURVE('',#567,#568,#275,.T.);
#689=EDGE_CURVE('',#569,#570,#315,.T.);
#690=EDGE_CURVE('',#571,#569,#316,.T.);
#691=EDGE_CURVE('',#572,#571,#317,.T.);
#692=EDGE_CURVE('',#572,#570,#318,.T.);
#693=EDGE_CURVE('',#570,#573,#319,.T.);
#694=EDGE_CURVE('',#572,#574,#320,.T.);
#695=EDGE_CURVE('',#573,#574,#321,.T.);
#696=EDGE_CURVE('',#575,#569,#322,.T.);
#697=EDGE_CURVE('',#576,#575,#323,.T.);
#698=EDGE_CURVE('',#571,#576,#324,.T.);
#699=EDGE_CURVE('',#577,#577,#508,.T.);
#700=EDGE_CURVE('',#573,#575,#509,.T.);
#701=EDGE_CURVE('',#576,#574,#510,.T.);
#702=EDGE_CURVE('',#577,#578,#325,.T.);
#703=EDGE_CURVE('',#578,#578,#511,.T.);
#704=EDGE_CURVE('',#579,#579,#512,.T.);
#705=EDGE_CURVE('',#580,#581,#326,.T.);
#706=EDGE_CURVE('',#582,#580,#327,.T.);
#707=EDGE_CURVE('',#582,#583,#328,.T.);
#708=EDGE_CURVE('',#581,#583,#329,.T.);
#709=EDGE_CURVE('',#584,#585,#330,.T.);
#710=EDGE_CURVE('',#586,#584,#331,.T.);
#711=EDGE_CURVE('',#586,#587,#332,.T.);
#712=EDGE_CURVE('',#585,#587,#333,.T.);
#713=EDGE_CURVE('',#583,#586,#513,.T.);
#714=EDGE_CURVE('',#588,#582,#514,.T.);
#715=EDGE_CURVE('',#587,#588,#515,.T.);
#716=EDGE_CURVE('',#584,#585,#516,.T.);
#717=EDGE_CURVE('',#580,#581,#517,.T.);
#718=EDGE_CURVE('',#579,#588,#334,.T.);
#719=EDGE_CURVE('',#589,#590,#335,.T.);
#720=EDGE_CURVE('',#591,#589,#336,.T.);
#721=EDGE_CURVE('',#592,#591,#337,.T.);
#722=EDGE_CURVE('',#590,#592,#338,.T.);
#723=EDGE_CURVE('',#592,#593,#339,.T.);
#724=EDGE_CURVE('',#594,#591,#340,.T.);
#725=EDGE_CURVE('',#593,#594,#341,.T.);
#726=EDGE_CURVE('',#595,#596,#342,.T.);
#727=EDGE_CURVE('',#593,#595,#343,.T.);
#728=EDGE_CURVE('',#596,#594,#344,.T.);
#729=EDGE_CURVE('',#596,#589,#518,.T.);
#730=EDGE_CURVE('',#595,#597,#519,.T.);
#731=EDGE_CURVE('',#597,#590,#520,.T.);
#732=EDGE_CURVE('',#597,#598,#345,.T.);
#733=EDGE_CURVE('',#598,#598,#521,.T.);
#734=EDGE_CURVE('',#599,#600,#346,.T.);
#735=EDGE_CURVE('',#600,#601,#347,.T.);
#736=EDGE_CURVE('',#601,#602,#348,.T.);
#737=EDGE_CURVE('',#599,#602,#349,.T.);
#738=EDGE_CURVE('',#600,#603,#350,.T.);
#739=EDGE_CURVE('',#603,#604,#351,.T.);
#740=EDGE_CURVE('',#604,#601,#352,.T.);
#741=EDGE_CURVE('',#605,#603,#353,.T.);
#742=EDGE_CURVE('',#605,#606,#354,.T.);
#743=EDGE_CURVE('',#606,#604,#355,.T.);
#744=EDGE_CURVE('',#599,#605,#356,.T.);
#745=EDGE_CURVE('',#602,#606,#357,.T.);
#746=EDGE_CURVE('',#607,#608,#358,.T.);
#747=EDGE_CURVE('',#609,#607,#359,.T.);
#748=EDGE_CURVE('',#609,#610,#360,.T.);
#749=EDGE_CURVE('',#610,#608,#361,.T.);
#750=EDGE_CURVE('',#608,#611,#522,.T.);
#751=EDGE_CURVE('',#612,#610,#362,.T.);
#752=EDGE_CURVE('',#611,#612,#363,.T.);
#753=EDGE_CURVE('',#613,#609,#364,.T.);
#754=EDGE_CURVE('',#613,#612,#365,.T.);
#755=EDGE_CURVE('',#611,#614,#366,.T.);
#756=EDGE_CURVE('',#614,#613,#367,.T.);
#757=EDGE_CURVE('',#615,#615,#523,.T.);
#758=EDGE_CURVE('',#615,#616,#368,.T.);
#759=EDGE_CURVE('',#616,#607,#524,.T.);
#760=EDGE_CURVE('',#614,#616,#525,.T.);
#761=EDGE_CURVE('',#617,#618,#369,.T.);
#762=EDGE_CURVE('',#617,#619,#370,.T.);
#763=EDGE_CURVE('',#620,#619,#371,.T.);
#764=EDGE_CURVE('',#618,#620,#372,.T.);
#765=EDGE_CURVE('',#618,#621,#373,.T.);
#766=EDGE_CURVE('',#622,#620,#374,.T.);
#767=EDGE_CURVE('',#621,#622,#375,.T.);
#768=EDGE_CURVE('',#623,#621,#376,.T.);
#769=EDGE_CURVE('',#624,#622,#377,.T.);
#770=EDGE_CURVE('',#623,#624,#378,.T.);
#771=EDGE_CURVE('',#617,#623,#379,.T.);
#772=EDGE_CURVE('',#619,#624,#380,.T.);
#773=ORIENTED_EDGE('',*,*,#625,.F.);
#774=ORIENTED_EDGE('',*,*,#626,.T.);
#775=ORIENTED_EDGE('',*,*,#627,.F.);
#776=ORIENTED_EDGE('',*,*,#626,.F.);
#777=ORIENTED_EDGE('',*,*,#628,.F.);
#778=ORIENTED_EDGE('',*,*,#629,.F.);
#779=ORIENTED_EDGE('',*,*,#630,.T.);
#780=ORIENTED_EDGE('',*,*,#631,.F.);
#781=ORIENTED_EDGE('',*,*,#632,.F.);
#782=ORIENTED_EDGE('',*,*,#633,.F.);
#783=ORIENTED_EDGE('',*,*,#634,.T.);
#784=ORIENTED_EDGE('',*,*,#629,.T.);
#785=ORIENTED_EDGE('',*,*,#625,.T.);
#786=ORIENTED_EDGE('',*,*,#635,.F.);
#787=ORIENTED_EDGE('',*,*,#636,.F.);
#788=ORIENTED_EDGE('',*,*,#637,.F.);
#789=ORIENTED_EDGE('',*,*,#633,.T.);
#790=ORIENTED_EDGE('',*,*,#638,.T.);
#791=ORIENTED_EDGE('',*,*,#630,.F.);
#792=ORIENTED_EDGE('',*,*,#634,.F.);
#793=ORIENTED_EDGE('',*,*,#637,.T.);
#794=ORIENTED_EDGE('',*,*,#631,.T.);
#795=ORIENTED_EDGE('',*,*,#638,.F.);
#796=ORIENTED_EDGE('',*,*,#636,.T.);
#797=ORIENTED_EDGE('',*,*,#639,.F.);
#798=ORIENTED_EDGE('',*,*,#640,.F.);
#799=ORIENTED_EDGE('',*,*,#641,.F.);
#800=ORIENTED_EDGE('',*,*,#642,.T.);
#801=ORIENTED_EDGE('',*,*,#643,.F.);
#802=ORIENTED_EDGE('',*,*,#644,.F.);
#803=ORIENTED_EDGE('',*,*,#645,.F.);
#804=ORIENTED_EDGE('',*,*,#646,.T.);
#805=ORIENTED_EDGE('',*,*,#647,.F.);
#806=ORIENTED_EDGE('',*,*,#648,.F.);
#807=ORIENTED_EDGE('',*,*,#642,.F.);
#808=ORIENTED_EDGE('',*,*,#649,.F.);
#809=ORIENTED_EDGE('',*,*,#646,.F.);
#810=ORIENTED_EDGE('',*,*,#644,.T.);
#811=ORIENTED_EDGE('',*,*,#650,.T.);
#812=ORIENTED_EDGE('',*,*,#640,.T.);
#813=ORIENTED_EDGE('',*,*,#651,.T.);
#814=ORIENTED_EDGE('',*,*,#652,.T.);
#815=ORIENTED_EDGE('',*,*,#653,.F.);
#816=ORIENTED_EDGE('',*,*,#654,.T.);
#817=ORIENTED_EDGE('',*,*,#655,.F.);
#818=ORIENTED_EDGE('',*,*,#654,.F.);
#819=ORIENTED_EDGE('',*,*,#627,.T.);
#820=ORIENTED_EDGE('',*,*,#653,.T.);
#821=ORIENTED_EDGE('',*,*,#628,.T.);
#822=ORIENTED_EDGE('',*,*,#639,.T.);
#823=ORIENTED_EDGE('',*,*,#635,.T.);
#824=ORIENTED_EDGE('',*,*,#632,.T.);
#825=ORIENTED_EDGE('',*,*,#656,.T.);
#826=ORIENTED_EDGE('',*,*,#655,.T.);
#827=ORIENTED_EDGE('',*,*,#656,.F.);
#828=ORIENTED_EDGE('',*,*,#657,.T.);
#829=ORIENTED_EDGE('',*,*,#651,.F.);
#830=ORIENTED_EDGE('',*,*,#643,.T.);
#831=ORIENTED_EDGE('',*,*,#648,.T.);
#832=ORIENTED_EDGE('',*,*,#645,.T.);
#833=ORIENTED_EDGE('',*,*,#650,.F.);
#834=ORIENTED_EDGE('',*,*,#647,.T.);
#835=ORIENTED_EDGE('',*,*,#649,.T.);
#836=ORIENTED_EDGE('',*,*,#641,.T.);
#837=ORIENTED_EDGE('',*,*,#652,.F.);
#838=ORIENTED_EDGE('',*,*,#657,.F.);
#839=ORIENTED_EDGE('',*,*,#658,.F.);
#840=ORIENTED_EDGE('',*,*,#659,.T.);
#841=ORIENTED_EDGE('',*,*,#660,.F.);
#842=ORIENTED_EDGE('',*,*,#661,.F.);
#843=ORIENTED_EDGE('',*,*,#662,.F.);
#844=ORIENTED_EDGE('',*,*,#663,.T.);
#845=ORIENTED_EDGE('',*,*,#664,.F.);
#846=ORIENTED_EDGE('',*,*,#665,.F.);
#847=ORIENTED_EDGE('',*,*,#666,.T.);
#848=ORIENTED_EDGE('',*,*,#664,.T.);
#849=ORIENTED_EDGE('',*,*,#667,.T.);
#850=ORIENTED_EDGE('',*,*,#668,.T.);
#851=ORIENTED_EDGE('',*,*,#660,.T.);
#852=ORIENTED_EDGE('',*,*,#658,.T.);
#853=ORIENTED_EDGE('',*,*,#669,.T.);
#854=ORIENTED_EDGE('',*,*,#662,.T.);
#855=ORIENTED_EDGE('',*,*,#670,.T.);
#856=ORIENTED_EDGE('',*,*,#671,.F.);
#857=ORIENTED_EDGE('',*,*,#672,.T.);
#858=ORIENTED_EDGE('',*,*,#673,.F.);
#859=ORIENTED_EDGE('',*,*,#674,.F.);
#860=ORIENTED_EDGE('',*,*,#675,.F.);
#861=ORIENTED_EDGE('',*,*,#676,.T.);
#862=ORIENTED_EDGE('',*,*,#677,.F.);
#863=ORIENTED_EDGE('',*,*,#678,.F.);
#864=ORIENTED_EDGE('',*,*,#679,.T.);
#865=ORIENTED_EDGE('',*,*,#677,.T.);
#866=ORIENTED_EDGE('',*,*,#680,.T.);
#867=ORIENTED_EDGE('',*,*,#673,.T.);
#868=ORIENTED_EDGE('',*,*,#671,.T.);
#869=ORIENTED_EDGE('',*,*,#681,.F.);
#870=ORIENTED_EDGE('',*,*,#675,.T.);
#871=ORIENTED_EDGE('',*,*,#682,.F.);
#872=ORIENTED_EDGE('',*,*,#683,.F.);
#873=ORIENTED_EDGE('',*,*,#667,.F.);
#874=ORIENTED_EDGE('',*,*,#663,.F.);
#875=ORIENTED_EDGE('',*,*,#670,.F.);
#876=ORIENTED_EDGE('',*,*,#665,.T.);
#877=ORIENTED_EDGE('',*,*,#666,.F.);
#878=ORIENTED_EDGE('',*,*,#659,.F.);
#879=ORIENTED_EDGE('',*,*,#669,.F.);
#880=ORIENTED_EDGE('',*,*,#661,.T.);
#881=ORIENTED_EDGE('',*,*,#668,.F.);
#882=ORIENTED_EDGE('',*,*,#684,.T.);
#883=ORIENTED_EDGE('',*,*,#682,.T.);
#884=ORIENTED_EDGE('',*,*,#678,.T.);
#885=ORIENTED_EDGE('',*,*,#679,.F.);
#886=ORIENTED_EDGE('',*,*,#672,.F.);
#887=ORIENTED_EDGE('',*,*,#681,.T.);
#888=ORIENTED_EDGE('',*,*,#674,.T.);
#889=ORIENTED_EDGE('',*,*,#680,.F.);
#890=ORIENTED_EDGE('',*,*,#676,.F.);
#891=ORIENTED_EDGE('',*,*,#683,.T.);
#892=ORIENTED_EDGE('',*,*,#684,.F.);
#893=ORIENTED_EDGE('',*,*,#685,.F.);
#894=ORIENTED_EDGE('',*,*,#686,.T.);
#895=ORIENTED_EDGE('',*,*,#687,.F.);
#896=ORIENTED_EDGE('',*,*,#688,.F.);
#897=ORIENTED_EDGE('',*,*,#686,.F.);
#898=ORIENTED_EDGE('',*,*,#689,.F.);
#899=ORIENTED_EDGE('',*,*,#690,.F.);
#900=ORIENTED_EDGE('',*,*,#691,.F.);
#901=ORIENTED_EDGE('',*,*,#692,.T.);
#902=ORIENTED_EDGE('',*,*,#685,.T.);
#903=ORIENTED_EDGE('',*,*,#693,.F.);
#904=ORIENTED_EDGE('',*,*,#692,.F.);
#905=ORIENTED_EDGE('',*,*,#694,.T.);
#906=ORIENTED_EDGE('',*,*,#695,.F.);
#907=ORIENTED_EDGE('',*,*,#696,.F.);
#908=ORIENTED_EDGE('',*,*,#697,.F.);
#909=ORIENTED_EDGE('',*,*,#698,.F.);
#910=ORIENTED_EDGE('',*,*,#690,.T.);
#911=ORIENTED_EDGE('',*,*,#699,.T.);
#912=ORIENTED_EDGE('',*,*,#696,.T.);
#913=ORIENTED_EDGE('',*,*,#689,.T.);
#914=ORIENTED_EDGE('',*,*,#693,.T.);
#915=ORIENTED_EDGE('',*,*,#700,.T.);
#916=ORIENTED_EDGE('',*,*,#697,.T.);
#917=ORIENTED_EDGE('',*,*,#700,.F.);
#918=ORIENTED_EDGE('',*,*,#695,.T.);
#919=ORIENTED_EDGE('',*,*,#701,.F.);
#920=ORIENTED_EDGE('',*,*,#699,.F.);
#921=ORIENTED_EDGE('',*,*,#702,.T.);
#922=ORIENTED_EDGE('',*,*,#703,.F.);
#923=ORIENTED_EDGE('',*,*,#702,.F.);
#924=ORIENTED_EDGE('',*,*,#687,.T.);
#925=ORIENTED_EDGE('',*,*,#688,.T.);
#926=ORIENTED_EDGE('',*,*,#704,.T.);
#927=ORIENTED_EDGE('',*,*,#703,.T.);
#928=ORIENTED_EDGE('',*,*,#705,.F.);
#929=ORIENTED_EDGE('',*,*,#706,.F.);
#930=ORIENTED_EDGE('',*,*,#707,.T.);
#931=ORIENTED_EDGE('',*,*,#708,.F.);
#932=ORIENTED_EDGE('',*,*,#709,.F.);
#933=ORIENTED_EDGE('',*,*,#710,.F.);
#934=ORIENTED_EDGE('',*,*,#711,.T.);
#935=ORIENTED_EDGE('',*,*,#712,.F.);
#936=ORIENTED_EDGE('',*,*,#713,.F.);
#937=ORIENTED_EDGE('',*,*,#707,.F.);
#938=ORIENTED_EDGE('',*,*,#714,.F.);
#939=ORIENTED_EDGE('',*,*,#715,.F.);
#940=ORIENTED_EDGE('',*,*,#711,.F.);
#941=ORIENTED_EDGE('',*,*,#709,.T.);
#942=ORIENTED_EDGE('',*,*,#716,.F.);
#943=ORIENTED_EDGE('',*,*,#705,.T.);
#944=ORIENTED_EDGE('',*,*,#717,.F.);
#945=ORIENTED_EDGE('',*,*,#704,.F.);
#946=ORIENTED_EDGE('',*,*,#718,.T.);
#947=ORIENTED_EDGE('',*,*,#714,.T.);
#948=ORIENTED_EDGE('',*,*,#706,.T.);
#949=ORIENTED_EDGE('',*,*,#717,.T.);
#950=ORIENTED_EDGE('',*,*,#708,.T.);
#951=ORIENTED_EDGE('',*,*,#713,.T.);
#952=ORIENTED_EDGE('',*,*,#710,.T.);
#953=ORIENTED_EDGE('',*,*,#716,.T.);
#954=ORIENTED_EDGE('',*,*,#712,.T.);
#955=ORIENTED_EDGE('',*,*,#715,.T.);
#956=ORIENTED_EDGE('',*,*,#718,.F.);
#957=ORIENTED_EDGE('',*,*,#701,.T.);
#958=ORIENTED_EDGE('',*,*,#694,.F.);
#959=ORIENTED_EDGE('',*,*,#691,.T.);
#960=ORIENTED_EDGE('',*,*,#698,.T.);
#961=ORIENTED_EDGE('',*,*,#719,.F.);
#962=ORIENTED_EDGE('',*,*,#720,.F.);
#963=ORIENTED_EDGE('',*,*,#721,.F.);
#964=ORIENTED_EDGE('',*,*,#722,.F.);
#965=ORIENTED_EDGE('',*,*,#723,.F.);
#966=ORIENTED_EDGE('',*,*,#721,.T.);
#967=ORIENTED_EDGE('',*,*,#724,.F.);
#968=ORIENTED_EDGE('',*,*,#725,.F.);
#969=ORIENTED_EDGE('',*,*,#726,.F.);
#970=ORIENTED_EDGE('',*,*,#727,.F.);
#971=ORIENTED_EDGE('',*,*,#725,.T.);
#972=ORIENTED_EDGE('',*,*,#728,.F.);
#973=ORIENTED_EDGE('',*,*,#729,.F.);
#974=ORIENTED_EDGE('',*,*,#728,.T.);
#975=ORIENTED_EDGE('',*,*,#724,.T.);
#976=ORIENTED_EDGE('',*,*,#720,.T.);
#977=ORIENTED_EDGE('',*,*,#722,.T.);
#978=ORIENTED_EDGE('',*,*,#723,.T.);
#979=ORIENTED_EDGE('',*,*,#727,.T.);
#980=ORIENTED_EDGE('',*,*,#730,.T.);
#981=ORIENTED_EDGE('',*,*,#731,.T.);
#982=ORIENTED_EDGE('',*,*,#730,.F.);
#983=ORIENTED_EDGE('',*,*,#726,.T.);
#984=ORIENTED_EDGE('',*,*,#729,.T.);
#985=ORIENTED_EDGE('',*,*,#719,.T.);
#986=ORIENTED_EDGE('',*,*,#731,.F.);
#987=ORIENTED_EDGE('',*,*,#732,.T.);
#988=ORIENTED_EDGE('',*,*,#733,.T.);
#989=ORIENTED_EDGE('',*,*,#732,.F.);
#990=ORIENTED_EDGE('',*,*,#733,.F.);
#991=ORIENTED_EDGE('',*,*,#734,.T.);
#992=ORIENTED_EDGE('',*,*,#735,.T.);
#993=ORIENTED_EDGE('',*,*,#736,.T.);
#994=ORIENTED_EDGE('',*,*,#737,.F.);
#995=ORIENTED_EDGE('',*,*,#738,.T.);
#996=ORIENTED_EDGE('',*,*,#739,.T.);
#997=ORIENTED_EDGE('',*,*,#740,.T.);
#998=ORIENTED_EDGE('',*,*,#735,.F.);
#999=ORIENTED_EDGE('',*,*,#741,.F.);
#1000=ORIENTED_EDGE('',*,*,#742,.T.);
#1001=ORIENTED_EDGE('',*,*,#743,.T.);
#1002=ORIENTED_EDGE('',*,*,#739,.F.);
#1003=ORIENTED_EDGE('',*,*,#744,.F.);
#1004=ORIENTED_EDGE('',*,*,#737,.T.);
#1005=ORIENTED_EDGE('',*,*,#745,.T.);
#1006=ORIENTED_EDGE('',*,*,#742,.F.);
#1007=ORIENTED_EDGE('',*,*,#745,.F.);
#1008=ORIENTED_EDGE('',*,*,#736,.F.);
#1009=ORIENTED_EDGE('',*,*,#740,.F.);
#1010=ORIENTED_EDGE('',*,*,#743,.F.);
#1011=ORIENTED_EDGE('',*,*,#744,.T.);
#1012=ORIENTED_EDGE('',*,*,#741,.T.);
#1013=ORIENTED_EDGE('',*,*,#738,.F.);
#1014=ORIENTED_EDGE('',*,*,#734,.F.);
#1015=ORIENTED_EDGE('',*,*,#746,.F.);
#1016=ORIENTED_EDGE('',*,*,#747,.F.);
#1017=ORIENTED_EDGE('',*,*,#748,.T.);
#1018=ORIENTED_EDGE('',*,*,#749,.T.);
#1019=ORIENTED_EDGE('',*,*,#750,.F.);
#1020=ORIENTED_EDGE('',*,*,#749,.F.);
#1021=ORIENTED_EDGE('',*,*,#751,.F.);
#1022=ORIENTED_EDGE('',*,*,#752,.F.);
#1023=ORIENTED_EDGE('',*,*,#753,.F.);
#1024=ORIENTED_EDGE('',*,*,#754,.T.);
#1025=ORIENTED_EDGE('',*,*,#751,.T.);
#1026=ORIENTED_EDGE('',*,*,#748,.F.);
#1027=ORIENTED_EDGE('',*,*,#755,.F.);
#1028=ORIENTED_EDGE('',*,*,#752,.T.);
#1029=ORIENTED_EDGE('',*,*,#754,.F.);
#1030=ORIENTED_EDGE('',*,*,#756,.F.);
#1031=ORIENTED_EDGE('',*,*,#757,.F.);
#1032=ORIENTED_EDGE('',*,*,#758,.T.);
#1033=ORIENTED_EDGE('',*,*,#759,.T.);
#1034=ORIENTED_EDGE('',*,*,#746,.T.);
#1035=ORIENTED_EDGE('',*,*,#750,.T.);
#1036=ORIENTED_EDGE('',*,*,#755,.T.);
#1037=ORIENTED_EDGE('',*,*,#760,.T.);
#1038=ORIENTED_EDGE('',*,*,#758,.F.);
#1039=ORIENTED_EDGE('',*,*,#757,.T.);
#1040=ORIENTED_EDGE('',*,*,#747,.T.);
#1041=ORIENTED_EDGE('',*,*,#759,.F.);
#1042=ORIENTED_EDGE('',*,*,#760,.F.);
#1043=ORIENTED_EDGE('',*,*,#756,.T.);
#1044=ORIENTED_EDGE('',*,*,#753,.T.);
#1045=ORIENTED_EDGE('',*,*,#761,.F.);
#1046=ORIENTED_EDGE('',*,*,#762,.T.);
#1047=ORIENTED_EDGE('',*,*,#763,.F.);
#1048=ORIENTED_EDGE('',*,*,#764,.F.);
#1049=ORIENTED_EDGE('',*,*,#765,.F.);
#1050=ORIENTED_EDGE('',*,*,#764,.T.);
#1051=ORIENTED_EDGE('',*,*,#766,.F.);
#1052=ORIENTED_EDGE('',*,*,#767,.F.);
#1053=ORIENTED_EDGE('',*,*,#768,.T.);
#1054=ORIENTED_EDGE('',*,*,#767,.T.);
#1055=ORIENTED_EDGE('',*,*,#769,.F.);
#1056=ORIENTED_EDGE('',*,*,#770,.F.);
#1057=ORIENTED_EDGE('',*,*,#771,.T.);
#1058=ORIENTED_EDGE('',*,*,#770,.T.);
#1059=ORIENTED_EDGE('',*,*,#772,.F.);
#1060=ORIENTED_EDGE('',*,*,#762,.F.);
#1061=ORIENTED_EDGE('',*,*,#772,.T.);
#1062=ORIENTED_EDGE('',*,*,#769,.T.);
#1063=ORIENTED_EDGE('',*,*,#766,.T.);
#1064=ORIENTED_EDGE('',*,*,#763,.T.);
#1065=ORIENTED_EDGE('',*,*,#771,.F.);
#1066=ORIENTED_EDGE('',*,*,#761,.T.);
#1067=ORIENTED_EDGE('',*,*,#765,.T.);
#1068=ORIENTED_EDGE('',*,*,#768,.F.);
#1069=CYLINDRICAL_SURFACE('',#1234,1.);
#1070=CYLINDRICAL_SURFACE('',#1241,4.);
#1071=CYLINDRICAL_SURFACE('',#1253,6.);
#1072=CYLINDRICAL_SURFACE('',#1259,12.5);
#1073=CYLINDRICAL_SURFACE('',#1281,12.5);
#1074=CYLINDRICAL_SURFACE('',#1283,0.999999999999999);
#1075=CYLINDRICAL_SURFACE('',#1291,4.);
#1076=CYLINDRICAL_SURFACE('',#1293,6.);
#1077=CYLINDRICAL_SURFACE('',#1307,12.5);
#1078=CYLINDRICAL_SURFACE('',#1318,4.);
#1079=CYLINDRICAL_SURFACE('',#1334,4.);
#1080=ADVANCED_FACE('',(#131),#1069,.F.);
#1081=ADVANCED_FACE('',(#132),#75,.F.);
#1082=ADVANCED_FACE('',(#133,#67),#76,.F.);
#1083=ADVANCED_FACE('',(#134),#77,.F.);
#1084=ADVANCED_FACE('',(#135),#78,.F.);
#1085=ADVANCED_FACE('',(#136),#1070,.F.);
#1086=ADVANCED_FACE('',(#137),#79,.F.);
#1087=ADVANCED_FACE('',(#138),#80,.F.);
#1088=ADVANCED_FACE('',(#139),#81,.T.);
#1089=ADVANCED_FACE('',(#140),#82,.T.);
#1090=ADVANCED_FACE('',(#141),#83,.T.);
#1091=ADVANCED_FACE('',(#142,#68),#1071,.T.);
#1092=ADVANCED_FACE('',(#143,#69),#84,.T.);
#1093=ADVANCED_FACE('',(#144,#70),#85,.F.);
#1094=ADVANCED_FACE('',(#145),#1072,.T.);
#1095=ADVANCED_FACE('',(#146),#86,.T.);
#1096=ADVANCED_FACE('',(#147),#87,.T.);
#1097=ADVANCED_FACE('',(#148),#88,.T.);
#1098=ADVANCED_FACE('',(#149),#89,.T.);
#1099=ADVANCED_FACE('',(#150),#90,.T.);
#1100=ADVANCED_FACE('',(#151),#91,.T.);
#1101=ADVANCED_FACE('',(#152),#92,.T.);
#1102=ADVANCED_FACE('',(#153),#93,.F.);
#1103=ADVANCED_FACE('',(#154),#94,.F.);
#1104=ADVANCED_FACE('',(#155),#95,.F.);
#1105=ADVANCED_FACE('',(#156),#1073,.T.);
#1106=ADVANCED_FACE('',(#157),#1074,.F.);
#1107=ADVANCED_FACE('',(#158,#71),#96,.T.);
#1108=ADVANCED_FACE('',(#159),#97,.T.);
#1109=ADVANCED_FACE('',(#160),#98,.T.);
#1110=ADVANCED_FACE('',(#161,#72),#99,.T.);
#1111=ADVANCED_FACE('',(#162),#1075,.F.);
#1112=ADVANCED_FACE('',(#163,#73),#1076,.T.);
#1113=ADVANCED_FACE('',(#164,#74),#100,.T.);
#1114=ADVANCED_FACE('',(#165),#101,.F.);
#1115=ADVANCED_FACE('',(#166),#102,.F.);
#1116=ADVANCED_FACE('',(#167),#103,.F.);
#1117=ADVANCED_FACE('',(#168),#104,.F.);
#1118=ADVANCED_FACE('',(#169),#105,.F.);
#1119=ADVANCED_FACE('',(#170),#1077,.T.);
#1120=ADVANCED_FACE('',(#171),#106,.T.);
#1121=ADVANCED_FACE('',(#172),#107,.T.);
#1122=ADVANCED_FACE('',(#173),#108,.T.);
#1123=ADVANCED_FACE('',(#174),#109,.T.);
#1124=ADVANCED_FACE('',(#175),#110,.T.);
#1125=ADVANCED_FACE('',(#176),#111,.T.);
#1126=ADVANCED_FACE('',(#177),#1078,.T.);
#1127=ADVANCED_FACE('',(#178),#112,.F.);
#1128=ADVANCED_FACE('',(#179),#113,.F.);
#1129=ADVANCED_FACE('',(#180),#114,.F.);
#1130=ADVANCED_FACE('',(#181),#115,.F.);
#1131=ADVANCED_FACE('',(#182),#116,.F.);
#1132=ADVANCED_FACE('',(#183),#117,.F.);
#1133=ADVANCED_FACE('',(#184),#118,.T.);
#1134=ADVANCED_FACE('',(#185),#119,.F.);
#1135=ADVANCED_FACE('',(#186),#120,.F.);
#1136=ADVANCED_FACE('',(#187),#121,.F.);
#1137=ADVANCED_FACE('',(#188),#122,.F.);
#1138=ADVANCED_FACE('',(#189),#1079,.T.);
#1139=ADVANCED_FACE('',(#190),#123,.T.);
#1140=ADVANCED_FACE('',(#191),#124,.F.);
#1141=ADVANCED_FACE('',(#192),#125,.T.);
#1142=ADVANCED_FACE('',(#193),#126,.T.);
#1143=ADVANCED_FACE('',(#194),#127,.T.);
#1144=ADVANCED_FACE('',(#195),#128,.T.);
#1145=ADVANCED_FACE('',(#196),#129,.T.);
#1146=ADVANCED_FACE('',(#197),#130,.F.);
#1147=CLOSED_SHELL('',(#1080,#1081,#1082,#1083,#1084,#1085,#1086,#1087,
#1088,#1089,#1090,#1091,#1092,#1093,#1094));
#1148=CLOSED_SHELL('',(#1095,#1096,#1097,#1098,#1099,#1100,#1101,#1102,
#1103,#1104,#1105));
#1149=CLOSED_SHELL('',(#1106,#1107,#1108,#1109,#1110,#1111,#1112,#1113,
#1114,#1115,#1116,#1117,#1118,#1119,#1120));
#1150=CLOSED_SHELL('',(#1121,#1122,#1123,#1124,#1125,#1126,#1127));
#1151=CLOSED_SHELL('',(#1128,#1129,#1130,#1131,#1132,#1133));
#1152=CLOSED_SHELL('',(#1134,#1135,#1136,#1137,#1138,#1139,#1140));
#1153=CLOSED_SHELL('',(#1141,#1142,#1143,#1144,#1145,#1146));
#1154=DERIVED_UNIT_ELEMENT(#1168,1.);
#1155=DERIVED_UNIT_ELEMENT(#2118,-3.);
#1156=DERIVED_UNIT_ELEMENT(#1168,1.);
#1157=DERIVED_UNIT_ELEMENT(#2118,-3.);
#1158=DERIVED_UNIT_ELEMENT(#1168,1.);
#1159=DERIVED_UNIT_ELEMENT(#2118,-3.);
#1160=DERIVED_UNIT_ELEMENT(#1168,1.);
#1161=DERIVED_UNIT_ELEMENT(#2118,-3.);
#1162=DERIVED_UNIT_ELEMENT(#1168,1.);
#1163=DERIVED_UNIT_ELEMENT(#2118,-3.);
#1164=DERIVED_UNIT_ELEMENT(#1168,1.);
#1165=DERIVED_UNIT_ELEMENT(#2118,-3.);
#1166=DERIVED_UNIT_ELEMENT(#1168,1.);
#1167=DERIVED_UNIT_ELEMENT(#2118,-3.);
#1168=(
MASS_UNIT()
NAMED_UNIT(*)
SI_UNIT(.KILO.,.GRAM.)
);
#1169=DERIVED_UNIT((#1154,#1155));
#1170=DERIVED_UNIT((#1156,#1157));
#1171=DERIVED_UNIT((#1158,#1159));
#1172=DERIVED_UNIT((#1160,#1161));
#1173=DERIVED_UNIT((#1162,#1163));
#1174=DERIVED_UNIT((#1164,#1165));
#1175=DERIVED_UNIT((#1166,#1167));
#1176=MEASURE_REPRESENTATION_ITEM('density measure',
POSITIVE_RATIO_MEASURE(7850.),#1169);
#1177=MEASURE_REPRESENTATION_ITEM('density measure',
POSITIVE_RATIO_MEASURE(7850.),#1170);
#1178=MEASURE_REPRESENTATION_ITEM('density measure',
POSITIVE_RATIO_MEASURE(7850.),#1171);
#1179=MEASURE_REPRESENTATION_ITEM('density measure',
POSITIVE_RATIO_MEASURE(7850.),#1172);
#1180=MEASURE_REPRESENTATION_ITEM('density measure',
POSITIVE_RATIO_MEASURE(7850.),#1173);
#1181=MEASURE_REPRESENTATION_ITEM('density measure',
POSITIVE_RATIO_MEASURE(7850.),#1174);
#1182=MEASURE_REPRESENTATION_ITEM('density measure',
POSITIVE_RATIO_MEASURE(7850.),#1175);
#1183=PROPERTY_DEFINITION_REPRESENTATION(#1218,#1197);
#1184=PROPERTY_DEFINITION_REPRESENTATION(#1219,#1198);
#1185=PROPERTY_DEFINITION_REPRESENTATION(#1220,#1199);
#1186=PROPERTY_DEFINITION_REPRESENTATION(#1221,#1200);
#1187=PROPERTY_DEFINITION_REPRESENTATION(#1222,#1201);
#1188=PROPERTY_DEFINITION_REPRESENTATION(#1223,#1202);
#1189=PROPERTY_DEFINITION_REPRESENTATION(#1224,#1203);
#1190=PROPERTY_DEFINITION_REPRESENTATION(#1225,#1204);
#1191=PROPERTY_DEFINITION_REPRESENTATION(#1226,#1205);
#1192=PROPERTY_DEFINITION_REPRESENTATION(#1227,#1206);
#1193=PROPERTY_DEFINITION_REPRESENTATION(#1228,#1207);
#1194=PROPERTY_DEFINITION_REPRESENTATION(#1229,#1208);
#1195=PROPERTY_DEFINITION_REPRESENTATION(#1230,#1209);
#1196=PROPERTY_DEFINITION_REPRESENTATION(#1231,#1210);
#1197=REPRESENTATION('material name',(#1211),#2109);
#1198=REPRESENTATION('density',(#1176),#2109);
#1199=REPRESENTATION('material name',(#1212),#2110);
#1200=REPRESENTATION('density',(#1177),#2110);
#1201=REPRESENTATION('material name',(#1213),#2111);
#1202=REPRESENTATION('density',(#1178),#2111);
#1203=REPRESENTATION('material name',(#1214),#2112);
#1204=REPRESENTATION('density',(#1179),#2112);
#1205=REPRESENTATION('material name',(#1215),#2113);
#1206=REPRESENTATION('density',(#1180),#2113);
#1207=REPRESENTATION('material name',(#1216),#2114);
#1208=REPRESENTATION('density',(#1181),#2114);
#1209=REPRESENTATION('material name',(#1217),#2115);
#1210=REPRESENTATION('density',(#1182),#2115);
#1211=DESCRIPTIVE_REPRESENTATION_ITEM('Steel','Steel');
#1212=DESCRIPTIVE_REPRESENTATION_ITEM('Steel','Steel');
#1213=DESCRIPTIVE_REPRESENTATION_ITEM('Steel','Steel');
#1214=DESCRIPTIVE_REPRESENTATION_ITEM('Steel','Steel');
#1215=DESCRIPTIVE_REPRESENTATION_ITEM('Steel','Steel');
#1216=DESCRIPTIVE_REPRESENTATION_ITEM('Steel','Steel');
#1217=DESCRIPTIVE_REPRESENTATION_ITEM('Steel','Steel');
#1218=PROPERTY_DEFINITION('material property','material name',#2154);
#1219=PROPERTY_DEFINITION('material property','density of part',#2154);
#1220=PROPERTY_DEFINITION('material property','material name',#2155);
#1221=PROPERTY_DEFINITION('material property','density of part',#2155);
#1222=PROPERTY_DEFINITION('material property','material name',#2156);
#1223=PROPERTY_DEFINITION('material property','density of part',#2156);
#1224=PROPERTY_DEFINITION('material property','material name',#2157);
#1225=PROPERTY_DEFINITION('material property','density of part',#2157);
#1226=PROPERTY_DEFINITION('material property','material name',#2158);
#1227=PROPERTY_DEFINITION('material property','density of part',#2158);
#1228=PROPERTY_DEFINITION('material property','material name',#2159);
#1229=PROPERTY_DEFINITION('material property','density of part',#2159);
#1230=PROPERTY_DEFINITION('material property','material name',#2160);
#1231=PROPERTY_DEFINITION('material property','density of part',#2160);
#1232=AXIS2_PLACEMENT_3D('',#1703,#1354,#1355);
#1233=AXIS2_PLACEMENT_3D('',#1704,#1356,#1357);
#1234=AXIS2_PLACEMENT_3D('',#1705,#1358,#1359);
#1235=AXIS2_PLACEMENT_3D('',#1707,#1360,#1361);
#1236=AXIS2_PLACEMENT_3D('',#1744,#1363,#1364);
#1237=AXIS2_PLACEMENT_3D('',#1753,#1369,#1370);
#1238=AXIS2_PLACEMENT_3D('',#1759,#1374,#1375);
#1239=AXIS2_PLACEMENT_3D('',#1765,#1379,#1380);
#1240=AXIS2_PLACEMENT_3D('',#1766,#1381,#1382);
#1241=AXIS2_PLACEMENT_3D('',#1767,#1383,#1384);
#1242=AXIS2_PLACEMENT_3D('',#1768,#1385,#1386);
#1243=AXIS2_PLACEMENT_3D('',#1769,#1387,#1388);
#1244=AXIS2_PLACEMENT_3D('',#1778,#1393,#1394);
#1245=AXIS2_PLACEMENT_3D('',#1787,#1399,#1400);
#1246=AXIS2_PLACEMENT_3D('',#1788,#1401,#1402);
#1247=AXIS2_PLACEMENT_3D('',#1789,#1403,#1404);
#1248=AXIS2_PLACEMENT_3D('',#1790,#1405,#1406);
#1249=AXIS2_PLACEMENT_3D('',#1791,#1407,#1408);
#1250=AXIS2_PLACEMENT_3D('',#1792,#1409,#1410);
#1251=AXIS2_PLACEMENT_3D('',#1794,#1411,#1412);
#1252=AXIS2_PLACEMENT_3D('',#1795,#1413,#1414);
#1253=AXIS2_PLACEMENT_3D('',#1796,#1415,#1416);
#1254=AXIS2_PLACEMENT_3D('',#1798,#1417,#1418);
#1255=AXIS2_PLACEMENT_3D('',#1801,#1420,#1421);
#1256=AXIS2_PLACEMENT_3D('',#1802,#1422,#1423);
#1257=AXIS2_PLACEMENT_3D('',#1803,#1424,#1425);
#1258=AXIS2_PLACEMENT_3D('',#1805,#1426,#1427);
#1259=AXIS2_PLACEMENT_3D('',#1806,#1428,#1429);
#1260=AXIS2_PLACEMENT_3D('',#1808,#1431,#1432);
#1261=AXIS2_PLACEMENT_3D('',#1809,#1433,#1434);
#1262=AXIS2_PLACEMENT_3D('',#1818,#1439,#1440);
#1263=AXIS2_PLACEMENT_3D('',#1827,#1445,#1446);
#1264=AXIS2_PLACEMENT_3D('',#1828,#1447,#1448);
#1265=AXIS2_PLACEMENT_3D('',#1830,#1449,#1450);
#1266=AXIS2_PLACEMENT_3D('',#1831,#1451,#1452);
#1267=AXIS2_PLACEMENT_3D('',#1832,#1453,#1454);
#1268=AXIS2_PLACEMENT_3D('',#1833,#1455,#1456);
#1269=AXIS2_PLACEMENT_3D('',#1834,#1457,#1458);
#1270=AXIS2_PLACEMENT_3D('',#1835,#1459,#1460);
#1271=AXIS2_PLACEMENT_3D('',#1836,#1461,#1462);
#1272=AXIS2_PLACEMENT_3D('',#1845,#1467,#1468);
#1273=AXIS2_PLACEMENT_3D('',#1854,#1473,#1474);
#1274=AXIS2_PLACEMENT_3D('',#1855,#1475,#1476);
#1275=AXIS2_PLACEMENT_3D('',#1856,#1477,#1478);
#1276=AXIS2_PLACEMENT_3D('',#1857,#1479,#1480);
#1277=AXIS2_PLACEMENT_3D('',#1858,#1481,#1482);
#1278=AXIS2_PLACEMENT_3D('',#1859,#1483,#1484);
#1279=AXIS2_PLACEMENT_3D('',#1861,#1485,#1486);
#1280=AXIS2_PLACEMENT_3D('',#1862,#1487,#1488);
#1281=AXIS2_PLACEMENT_3D('',#1863,#1489,#1490);
#1282=AXIS2_PLACEMENT_3D('',#1865,#1492,#1493);
#1283=AXIS2_PLACEMENT_3D('',#1866,#1494,#1495);
#1284=AXIS2_PLACEMENT_3D('',#1868,#1496,#1497);
#1285=AXIS2_PLACEMENT_3D('',#1908,#1499,#1500);
#1286=AXIS2_PLACEMENT_3D('',#1917,#1505,#1506);
#1287=AXIS2_PLACEMENT_3D('',#1923,#1510,#1511);
#1288=AXIS2_PLACEMENT_3D('',#1929,#1515,#1516);
#1289=AXIS2_PLACEMENT_3D('',#1931,#1517,#1518);
#1290=AXIS2_PLACEMENT_3D('',#1932,#1519,#1520);
#1291=AXIS2_PLACEMENT_3D('',#1933,#1521,#1522);
#1292=AXIS2_PLACEMENT_3D('',#1934,#1523,#1524);
#1293=AXIS2_PLACEMENT_3D('',#1935,#1525,#1526);
#1294=AXIS2_PLACEMENT_3D('',#1938,#1528,#1529);
#1295=AXIS2_PLACEMENT_3D('',#1939,#1530,#1531);
#1296=AXIS2_PLACEMENT_3D('',#1941,#1532,#1533);
#1297=AXIS2_PLACEMENT_3D('',#1942,#1534,#1535);
#1298=AXIS2_PLACEMENT_3D('',#1951,#1540,#1541);
#1299=AXIS2_PLACEMENT_3D('',#1960,#1546,#1547);
#1300=AXIS2_PLACEMENT_3D('',#1961,#1548,#1549);
#1301=AXIS2_PLACEMENT_3D('',#1963,#1550,#1551);
#1302=AXIS2_PLACEMENT_3D('',#1964,#1552,#1553);
#1303=AXIS2_PLACEMENT_3D('',#1965,#1554,#1555);
#1304=AXIS2_PLACEMENT_3D('',#1966,#1556,#1557);
#1305=AXIS2_PLACEMENT_3D('',#1967,#1558,#1559);
#1306=AXIS2_PLACEMENT_3D('',#1968,#1560,#1561);
#1307=AXIS2_PLACEMENT_3D('',#1969,#1562,#1563);
#1308=AXIS2_PLACEMENT_3D('',#1971,#1565,#1566);
#1309=AXIS2_PLACEMENT_3D('',#1972,#1567,#1568);
#1310=AXIS2_PLACEMENT_3D('',#1973,#1569,#1570);
#1311=AXIS2_PLACEMENT_3D('',#1982,#1575,#1576);
#1312=AXIS2_PLACEMENT_3D('',#1988,#1580,#1581);
#1313=AXIS2_PLACEMENT_3D('',#1994,#1585,#1586);
#1314=AXIS2_PLACEMENT_3D('',#1995,#1587,#1588);
#1315=AXIS2_PLACEMENT_3D('',#1996,#1589,#1590);
#1316=AXIS2_PLACEMENT_3D('',#1998,#1591,#1592);
#1317=AXIS2_PLACEMENT_3D('',#1999,#1593,#1594);
#1318=AXIS2_PLACEMENT_3D('',#2000,#1595,#1596);
#1319=AXIS2_PLACEMENT_3D('',#2003,#1598,#1599);
#1320=AXIS2_PLACEMENT_3D('',#2004,#1600,#1601);
#1321=AXIS2_PLACEMENT_3D('',#2005,#1602,#1603);
#1322=AXIS2_PLACEMENT_3D('',#2006,#1604,#1605);
#1323=AXIS2_PLACEMENT_3D('',#2015,#1610,#1611);
#1324=AXIS2_PLACEMENT_3D('',#2021,#1615,#1616);
#1325=AXIS2_PLACEMENT_3D('',#2027,#1620,#1621);
#1326=AXIS2_PLACEMENT_3D('',#2030,#1624,#1625);
#1327=AXIS2_PLACEMENT_3D('',#2031,#1626,#1627);
#1328=AXIS2_PLACEMENT_3D('',#2032,#1628,#1629);
#1329=AXIS2_PLACEMENT_3D('',#2033,#1630,#1631);
#1330=AXIS2_PLACEMENT_3D('',#2042,#1636,#1637);
#1331=AXIS2_PLACEMENT_3D('',#2044,#1638,#1639);
#1332=AXIS2_PLACEMENT_3D('',#2048,#1642,#1643);
#1333=AXIS2_PLACEMENT_3D('',#2052,#1646,#1647);
#1334=AXIS2_PLACEMENT_3D('',#2056,#1650,#1651);
#1335=AXIS2_PLACEMENT_3D('',#2058,#1652,#1653);
#1336=AXIS2_PLACEMENT_3D('',#2061,#1655,#1656);
#1337=AXIS2_PLACEMENT_3D('',#2062,#1657,#1658);
#1338=AXIS2_PLACEMENT_3D('',#2063,#1659,#1660);
#1339=AXIS2_PLACEMENT_3D('',#2064,#1661,#1662);
#1340=AXIS2_PLACEMENT_3D('',#2065,#1663,#1664);
#1341=AXIS2_PLACEMENT_3D('',#2066,#1665,#1666);
#1342=AXIS2_PLACEMENT_3D('',#2075,#1671,#1672);
#1343=AXIS2_PLACEMENT_3D('',#2081,#1676,#1677);
#1344=AXIS2_PLACEMENT_3D('',#2087,#1681,#1682);
#1345=AXIS2_PLACEMENT_3D('',#2090,#1685,#1686);
#1346=AXIS2_PLACEMENT_3D('',#2091,#1687,#1688);
#1347=AXIS2_PLACEMENT_3D('',#2092,#1689,#1690);
#1348=AXIS2_PLACEMENT_3D('',#2093,#1691,#1692);
#1349=AXIS2_PLACEMENT_3D('',#2094,#1693,#1694);
#1350=AXIS2_PLACEMENT_3D('',#2095,#1695,#1696);
#1351=AXIS2_PLACEMENT_3D('',#2096,#1697,#1698);
#1352=AXIS2_PLACEMENT_3D('',#2097,#1699,#1700);
#1353=AXIS2_PLACEMENT_3D('',#2098,#1701,#1702);
#1354=DIRECTION('axis',(0.,0.,1.));
#1355=DIRECTION('refdir',(1.,0.,0.));
#1356=DIRECTION('axis',(0.,0.,1.));
#1357=DIRECTION('refdir',(1.,0.,0.));
#1358=DIRECTION('center_axis',(0.,0.,1.));
#1359=DIRECTION('ref_axis',(1.,0.,0.));
#1360=DIRECTION('center_axis',(0.,0.,1.));
#1361=DIRECTION('ref_axis',(1.,0.,0.));
#1362=DIRECTION('',(0.,0.,1.));
#1363=DIRECTION('center_axis',(1.,0.,0.));
#1364=DIRECTION('ref_axis',(0.,0.,1.));
#1365=DIRECTION('',(0.,0.,-1.));
#1366=DIRECTION('',(0.,-1.,0.));
#1367=DIRECTION('',(0.,0.,-1.));
#1368=DIRECTION('',(0.,1.,0.));
#1369=DIRECTION('center_axis',(0.,0.,1.));
#1370=DIRECTION('ref_axis',(-1.,0.,0.));
#1371=DIRECTION('',(1.,0.,0.));
#1372=DIRECTION('',(0.,-1.,0.));
#1373=DIRECTION('',(1.,0.,0.));
#1374=DIRECTION('center_axis',(-1.,0.,0.));
#1375=DIRECTION('ref_axis',(0.,0.,-1.));
#1376=DIRECTION('',(0.,0.,1.));
#1377=DIRECTION('',(0.,-1.,0.));
#1378=DIRECTION('',(0.,0.,-1.));
#1379=DIRECTION('center_axis',(0.,1.,0.));
#1380=DIRECTION('ref_axis',(1.,0.,0.));
#1381=DIRECTION('center_axis',(0.,-1.,0.));
#1382=DIRECTION('ref_axis',(1.,0.,0.));
#1383=DIRECTION('center_axis',(0.,-1.,0.));
#1384=DIRECTION('ref_axis',(6.12323399573677E-17,0.,-1.));
#1385=DIRECTION('center_axis',(0.,1.,0.));
#1386=DIRECTION('ref_axis',(1.,0.,0.));
#1387=DIRECTION('center_axis',(-1.,0.,0.));
#1388=DIRECTION('ref_axis',(0.,0.,-1.));
#1389=DIRECTION('',(0.,0.,-1.));
#1390=DIRECTION('',(0.,1.,0.));
#1391=DIRECTION('',(0.,0.,-1.));
#1392=DIRECTION('',(0.,-1.,0.));
#1393=DIRECTION('center_axis',(1.,0.,0.));
#1394=DIRECTION('ref_axis',(0.,0.,1.));
#1395=DIRECTION('',(0.,0.,1.));
#1396=DIRECTION('',(0.,1.,0.));
#1397=DIRECTION('',(0.,0.,1.));
#1398=DIRECTION('',(0.,-1.,0.));
#1399=DIRECTION('center_axis',(0.,1.,0.));
#1400=DIRECTION('ref_axis',(-1.,0.,0.));
#1401=DIRECTION('center_axis',(0.,-1.,0.));
#1402=DIRECTION('ref_axis',(1.,0.,0.));
#1403=DIRECTION('center_axis',(0.,-1.,0.));
#1404=DIRECTION('ref_axis',(1.,0.,0.));
#1405=DIRECTION('center_axis',(0.,1.,0.));
#1406=DIRECTION('ref_axis',(1.,0.,0.));
#1407=DIRECTION('center_axis',(0.,1.,0.));
#1408=DIRECTION('ref_axis',(1.,0.,0.));
#1409=DIRECTION('center_axis',(0.,1.,0.));
#1410=DIRECTION('ref_axis',(1.,0.,0.));
#1411=DIRECTION('center_axis',(0.,1.,0.));
#1412=DIRECTION('ref_axis',(1.,0.,0.));
#1413=DIRECTION('center_axis',(0.,1.,0.));
#1414=DIRECTION('ref_axis',(1.,0.,0.));
#1415=DIRECTION('center_axis',(0.,-1.,0.));
#1416=DIRECTION('ref_axis',(1.,0.,0.));
#1417=DIRECTION('center_axis',(0.,-1.,0.));
#1418=DIRECTION('ref_axis',(1.,0.,0.));
#1419=DIRECTION('',(0.,1.,0.));
#1420=DIRECTION('center_axis',(0.,1.,0.));
#1421=DIRECTION('ref_axis',(1.,0.,0.));
#1422=DIRECTION('center_axis',(0.,-1.,0.));
#1423=DIRECTION('ref_axis',(1.,0.,0.));
#1424=DIRECTION('center_axis',(0.,1.,0.));
#1425=DIRECTION('ref_axis',(1.,0.,0.));
#1426=DIRECTION('center_axis',(0.,-1.,0.));
#1427=DIRECTION('ref_axis',(1.,0.,0.));
#1428=DIRECTION('center_axis',(0.,-1.,0.));
#1429=DIRECTION('ref_axis',(1.,0.,0.));
#1430=DIRECTION('',(0.,1.,0.));
#1431=DIRECTION('axis',(0.,0.,1.));
#1432=DIRECTION('refdir',(1.,0.,0.));
#1433=DIRECTION('center_axis',(0.,0.,-1.));
#1434=DIRECTION('ref_axis',(-1.,0.,0.));
#1435=DIRECTION('',(1.,0.,0.));
#1436=DIRECTION('',(0.,1.,0.));
#1437=DIRECTION('',(-1.,0.,0.));
#1438=DIRECTION('',(0.,1.,0.));
#1439=DIRECTION('center_axis',(0.,0.,1.));
#1440=DIRECTION('ref_axis',(1.,0.,0.));
#1441=DIRECTION('',(-1.,0.,0.));
#1442=DIRECTION('',(0.,1.,0.));
#1443=DIRECTION('',(1.,0.,0.));
#1444=DIRECTION('',(0.,1.,0.));
#1445=DIRECTION('center_axis',(0.,1.,0.));
#1446=DIRECTION('ref_axis',(-1.,0.,0.));
#1447=DIRECTION('center_axis',(0.,1.,0.));
#1448=DIRECTION('ref_axis',(-1.,0.,0.));
#1449=DIRECTION('center_axis',(0.,1.,0.));
#1450=DIRECTION('ref_axis',(-1.,0.,0.));
#1451=DIRECTION('center_axis',(0.,1.,0.));
#1452=DIRECTION('ref_axis',(-1.,0.,0.));
#1453=DIRECTION('center_axis',(0.,1.,0.));
#1454=DIRECTION('ref_axis',(-1.,0.,0.));
#1455=DIRECTION('center_axis',(0.,1.,0.));
#1456=DIRECTION('ref_axis',(-1.,0.,0.));
#1457=DIRECTION('center_axis',(0.,1.,0.));
#1458=DIRECTION('ref_axis',(-1.,0.,0.));
#1459=DIRECTION('center_axis',(0.,1.,0.));
#1460=DIRECTION('ref_axis',(-1.,0.,0.));
#1461=DIRECTION('center_axis',(-1.,0.,0.));
#1462=DIRECTION('ref_axis',(0.,0.,-1.));
#1463=DIRECTION('',(0.,0.,1.));
#1464=DIRECTION('',(0.,-1.,0.));
#1465=DIRECTION('',(0.,0.,-1.));
#1466=DIRECTION('',(0.,-1.,0.));
#1467=DIRECTION('center_axis',(1.,0.,0.));
#1468=DIRECTION('ref_axis',(0.,0.,1.));
#1469=DIRECTION('',(0.,0.,-1.));
#1470=DIRECTION('',(0.,-1.,0.));
#1471=DIRECTION('',(0.,0.,1.));
#1472=DIRECTION('',(0.,-1.,0.));
#1473=DIRECTION('center_axis',(0.,1.,0.));
#1474=DIRECTION('ref_axis',(-1.,0.,0.));
#1475=DIRECTION('center_axis',(0.,-1.,0.));
#1476=DIRECTION('ref_axis',(-1.,0.,0.));
#1477=DIRECTION('center_axis',(0.,-1.,0.));
#1478=DIRECTION('ref_axis',(-1.,0.,0.));
#1479=DIRECTION('center_axis',(0.,1.,0.));
#1480=DIRECTION('ref_axis',(-1.,0.,0.));
#1481=DIRECTION('center_axis',(0.,1.,0.));
#1482=DIRECTION('ref_axis',(-1.,0.,0.));
#1483=DIRECTION('center_axis',(0.,1.,0.));
#1484=DIRECTION('ref_axis',(-1.,0.,0.));
#1485=DIRECTION('center_axis',(0.,1.,0.));
#1486=DIRECTION('ref_axis',(-1.,0.,0.));
#1487=DIRECTION('center_axis',(0.,1.,0.));
#1488=DIRECTION('ref_axis',(-1.,0.,0.));
#1489=DIRECTION('center_axis',(0.,1.,0.));
#1490=DIRECTION('ref_axis',(-1.,0.,0.));
#1491=DIRECTION('',(0.,-1.,0.));
#1492=DIRECTION('axis',(0.,0.,1.));
#1493=DIRECTION('refdir',(1.,0.,0.));
#1494=DIRECTION('center_axis',(0.,0.,1.));
#1495=DIRECTION('ref_axis',(1.,0.,0.));
#1496=DIRECTION('center_axis',(0.,0.,1.));
#1497=DIRECTION('ref_axis',(1.,0.,0.));
#1498=DIRECTION('',(0.,0.,1.));
#1499=DIRECTION('center_axis',(0.,0.,-1.));
#1500=DIRECTION('ref_axis',(-1.,0.,0.));
#1501=DIRECTION('',(-1.,0.,0.));
#1502=DIRECTION('',(0.,1.,0.));
#1503=DIRECTION('',(1.,0.,0.));
#1504=DIRECTION('',(0.,1.,0.));
#1505=DIRECTION('center_axis',(1.,0.,0.));
#1506=DIRECTION('ref_axis',(0.,0.,-1.));
#1507=DIRECTION('',(0.,0.,-1.));
#1508=DIRECTION('',(0.,0.,-1.));
#1509=DIRECTION('',(0.,-1.,0.));
#1510=DIRECTION('center_axis',(-1.,0.,0.));
#1511=DIRECTION('ref_axis',(0.,0.,1.));
#1512=DIRECTION('',(0.,0.,1.));
#1513=DIRECTION('',(0.,1.,0.));
#1514=DIRECTION('',(0.,0.,-1.));
#1515=DIRECTION('center_axis',(0.,1.,0.));
#1516=DIRECTION('ref_axis',(-1.,0.,0.));
#1517=DIRECTION('center_axis',(0.,1.,0.));
#1518=DIRECTION('ref_axis',(-1.,0.,0.));
#1519=DIRECTION('center_axis',(0.,-1.,0.));
#1520=DIRECTION('ref_axis',(-1.,0.,0.));
#1521=DIRECTION('center_axis',(0.,1.,0.));
#1522=DIRECTION('ref_axis',(1.83697019872103E-16,0.,-1.));
#1523=DIRECTION('center_axis',(0.,1.,0.));
#1524=DIRECTION('ref_axis',(-1.,0.,0.));
#1525=DIRECTION('center_axis',(0.,1.,0.));
#1526=DIRECTION('ref_axis',(-1.,0.,0.));
#1527=DIRECTION('',(0.,-1.,0.));
#1528=DIRECTION('center_axis',(0.,-1.,0.));
#1529=DIRECTION('ref_axis',(-1.,0.,0.));
#1530=DIRECTION('center_axis',(0.,1.,0.));
#1531=DIRECTION('ref_axis',(-1.,0.,0.));
#1532=DIRECTION('center_axis',(0.,1.,0.));
#1533=DIRECTION('ref_axis',(-1.,0.,0.));
#1534=DIRECTION('center_axis',(0.,0.,-1.));
#1535=DIRECTION('ref_axis',(-1.,0.,0.));
#1536=DIRECTION('',(-1.,0.,0.));
#1537=DIRECTION('',(0.,-1.,0.));
#1538=DIRECTION('',(-1.,0.,0.));
#1539=DIRECTION('',(0.,1.,0.));
#1540=DIRECTION('center_axis',(0.,0.,1.));
#1541=DIRECTION('ref_axis',(1.,0.,0.));
#1542=DIRECTION('',(1.,0.,0.));
#1543=DIRECTION('',(0.,-1.,0.));
#1544=DIRECTION('',(1.,0.,0.));
#1545=DIRECTION('',(0.,1.,0.));
#1546=DIRECTION('center_axis',(0.,1.,0.));
#1547=DIRECTION('ref_axis',(-1.,0.,0.));
#1548=DIRECTION('center_axis',(0.,1.,0.));
#1549=DIRECTION('ref_axis',(-1.,0.,0.));
#1550=DIRECTION('center_axis',(0.,1.,0.));
#1551=DIRECTION('ref_axis',(-1.,0.,0.));
#1552=DIRECTION('center_axis',(0.,1.,0.));
#1553=DIRECTION('ref_axis',(-1.,0.,0.));
#1554=DIRECTION('center_axis',(0.,1.,0.));
#1555=DIRECTION('ref_axis',(-1.,0.,0.));
#1556=DIRECTION('center_axis',(0.,1.,0.));
#1557=DIRECTION('ref_axis',(-1.,0.,0.));
#1558=DIRECTION('center_axis',(0.,1.,0.));
#1559=DIRECTION('ref_axis',(-1.,0.,0.));
#1560=DIRECTION('center_axis',(0.,1.,0.));
#1561=DIRECTION('ref_axis',(-1.,0.,0.));
#1562=DIRECTION('center_axis',(0.,1.,0.));
#1563=DIRECTION('ref_axis',(-1.,0.,0.));
#1564=DIRECTION('',(0.,-1.,0.));
#1565=DIRECTION('center_axis',(0.,1.,0.));
#1566=DIRECTION('ref_axis',(-1.,0.,0.));
#1567=DIRECTION('axis',(0.,0.,1.));
#1568=DIRECTION('refdir',(1.,0.,0.));
#1569=DIRECTION('center_axis',(-1.,0.,0.));
#1570=DIRECTION('ref_axis',(0.,0.,1.));
#1571=DIRECTION('',(0.,-1.,0.));
#1572=DIRECTION('',(0.,0.,1.));
#1573=DIRECTION('',(0.,1.,0.));
#1574=DIRECTION('',(0.,0.,-1.));
#1575=DIRECTION('center_axis',(0.,0.,1.));
#1576=DIRECTION('ref_axis',(1.,0.,0.));
#1577=DIRECTION('',(-1.,0.,0.));
#1578=DIRECTION('',(1.,0.,0.));
#1579=DIRECTION('',(0.,1.,0.));
#1580=DIRECTION('center_axis',(1.,0.,0.));
#1581=DIRECTION('ref_axis',(0.,0.,-1.));
#1582=DIRECTION('',(0.,1.,0.));
#1583=DIRECTION('',(0.,0.,1.));
#1584=DIRECTION('',(0.,0.,-1.));
#1585=DIRECTION('center_axis',(0.,-1.,0.));
#1586=DIRECTION('ref_axis',(0.,0.,-1.));
#1587=DIRECTION('center_axis',(0.,1.,0.));
#1588=DIRECTION('ref_axis',(1.,0.,0.));
#1589=DIRECTION('center_axis',(0.,-1.,0.));
#1590=DIRECTION('ref_axis',(1.,0.,0.));
#1591=DIRECTION('center_axis',(0.,-1.,0.));
#1592=DIRECTION('ref_axis',(1.,0.,0.));
#1593=DIRECTION('center_axis',(0.,-1.,0.));
#1594=DIRECTION('ref_axis',(1.,0.,0.));
#1595=DIRECTION('center_axis',(0.,-1.,0.));
#1596=DIRECTION('ref_axis',(1.,0.,0.));
#1597=DIRECTION('',(0.,1.,0.));
#1598=DIRECTION('center_axis',(0.,-1.,0.));
#1599=DIRECTION('ref_axis',(1.,0.,0.));
#1600=DIRECTION('center_axis',(0.,-1.,0.));
#1601=DIRECTION('ref_axis',(1.,0.,0.));
#1602=DIRECTION('axis',(0.,0.,1.));
#1603=DIRECTION('refdir',(1.,0.,0.));
#1604=DIRECTION('center_axis',(0.,0.,-1.));
#1605=DIRECTION('ref_axis',(-1.,0.,0.));
#1606=DIRECTION('',(1.,0.,0.));
#1607=DIRECTION('',(0.,1.,0.));
#1608=DIRECTION('',(-1.,0.,0.));
#1609=DIRECTION('',(0.,1.,0.));
#1610=DIRECTION('center_axis',(-1.,0.,0.));
#1611=DIRECTION('ref_axis',(0.,0.,1.));
#1612=DIRECTION('',(0.,0.,-1.));
#1613=DIRECTION('',(0.,1.,0.));
#1614=DIRECTION('',(0.,0.,1.));
#1615=DIRECTION('center_axis',(0.,0.,1.));
#1616=DIRECTION('ref_axis',(1.,0.,0.));
#1617=DIRECTION('',(1.,0.,0.));
#1618=DIRECTION('',(0.,1.,0.));
#1619=DIRECTION('',(1.,0.,0.));
#1620=DIRECTION('center_axis',(1.,0.,0.));
#1621=DIRECTION('ref_axis',(0.,0.,-1.));
#1622=DIRECTION('',(0.,0.,-1.));
#1623=DIRECTION('',(0.,0.,-1.));
#1624=DIRECTION('center_axis',(0.,-1.,0.));
#1625=DIRECTION('ref_axis',(0.,0.,-1.));
#1626=DIRECTION('center_axis',(0.,-1.,0.));
#1627=DIRECTION('ref_axis',(1.,0.,0.));
#1628=DIRECTION('axis',(0.,0.,1.));
#1629=DIRECTION('refdir',(1.,0.,0.));
#1630=DIRECTION('center_axis',(1.,0.,0.));
#1631=DIRECTION('ref_axis',(0.,0.,1.));
#1632=DIRECTION('',(0.,-1.,0.));
#1633=DIRECTION('',(0.,0.,1.));
#1634=DIRECTION('',(0.,-1.,0.));
#1635=DIRECTION('',(0.,0.,1.));
#1636=DIRECTION('center_axis',(0.,-1.,0.));
#1637=DIRECTION('ref_axis',(0.,0.,-1.));
#1638=DIRECTION('center_axis',(0.,-1.,0.));
#1639=DIRECTION('ref_axis',(1.,0.,0.));
#1640=DIRECTION('',(1.,0.,0.));
#1641=DIRECTION('',(0.,0.,-1.));
#1642=DIRECTION('center_axis',(0.,0.,-1.));
#1643=DIRECTION('ref_axis',(1.,0.,0.));
#1644=DIRECTION('',(1.,0.,0.));
#1645=DIRECTION('',(0.,-1.,0.));
#1646=DIRECTION('center_axis',(-1.,0.,0.));
#1647=DIRECTION('ref_axis',(0.,0.,-1.));
#1648=DIRECTION('',(0.,1.,0.));
#1649=DIRECTION('',(0.,0.,-1.));
#1650=DIRECTION('center_axis',(0.,-1.,0.));
#1651=DIRECTION('ref_axis',(1.,0.,0.));
#1652=DIRECTION('center_axis',(0.,-1.,0.));
#1653=DIRECTION('ref_axis',(1.,0.,0.));
#1654=DIRECTION('',(0.,1.,0.));
#1655=DIRECTION('center_axis',(0.,-1.,0.));
#1656=DIRECTION('ref_axis',(1.,0.,0.));
#1657=DIRECTION('center_axis',(0.,-1.,0.));
#1658=DIRECTION('ref_axis',(1.,0.,0.));
#1659=DIRECTION('center_axis',(0.,-1.,0.));
#1660=DIRECTION('ref_axis',(1.,0.,0.));
#1661=DIRECTION('center_axis',(0.,-1.,0.));
#1662=DIRECTION('ref_axis',(1.,0.,0.));
#1663=DIRECTION('axis',(0.,0.,1.));
#1664=DIRECTION('refdir',(1.,0.,0.));
#1665=DIRECTION('center_axis',(0.,0.,1.));
#1666=DIRECTION('ref_axis',(-1.,0.,0.));
#1667=DIRECTION('',(1.,0.,0.));
#1668=DIRECTION('',(0.,-1.,0.));
#1669=DIRECTION('',(-1.,0.,0.));
#1670=DIRECTION('',(0.,-1.,0.));
#1671=DIRECTION('center_axis',(1.,0.,0.));
#1672=DIRECTION('ref_axis',(0.,0.,1.));
#1673=DIRECTION('',(0.,0.,-1.));
#1674=DIRECTION('',(0.,0.,1.));
#1675=DIRECTION('',(0.,-1.,0.));
#1676=DIRECTION('center_axis',(0.,0.,-1.));
#1677=DIRECTION('ref_axis',(1.,0.,0.));
#1678=DIRECTION('',(1.,0.,0.));
#1679=DIRECTION('',(1.,0.,0.));
#1680=DIRECTION('',(0.,-1.,0.));
#1681=DIRECTION('center_axis',(-1.,0.,0.));
#1682=DIRECTION('ref_axis',(0.,0.,-1.));
#1683=DIRECTION('',(0.,0.,-1.));
#1684=DIRECTION('',(0.,0.,-1.));
#1685=DIRECTION('center_axis',(0.,-1.,0.));
#1686=DIRECTION('ref_axis',(0.,0.,-1.));
#1687=DIRECTION('center_axis',(0.,-1.,0.));
#1688=DIRECTION('ref_axis',(1.,0.,0.));
#1689=DIRECTION('',(0.,0.,1.));
#1690=DIRECTION('',(1.,0.,0.));
#1691=DIRECTION('',(0.,0.,1.));
#1692=DIRECTION('',(1.,0.,0.));
#1693=DIRECTION('',(0.,0.,1.));
#1694=DIRECTION('',(1.,0.,0.));
#1695=DIRECTION('',(0.,0.,1.));
#1696=DIRECTION('',(1.,0.,0.));
#1697=DIRECTION('',(-6.12323399573677E-17,0.,1.));
#1698=DIRECTION('',(1.,0.,6.12323399573677E-17));
#1699=DIRECTION('',(0.,0.,1.));
#1700=DIRECTION('',(1.,0.,0.));
#1701=DIRECTION('',(0.,0.,1.));
#1702=DIRECTION('',(1.,0.,0.));
#1703=CARTESIAN_POINT('',(0.,0.,0.));
#1704=CARTESIAN_POINT('',(0.,0.,0.));
#1705=CARTESIAN_POINT('Origin',(0.,-8.,0.));
#1706=CARTESIAN_POINT('',(-1.,-8.,4.84122918275927));
#1707=CARTESIAN_POINT('Origin',(0.,-8.,4.84122918275927));
#1708=CARTESIAN_POINT('',(-1.,-8.,5.91607978309962));
#1709=CARTESIAN_POINT('',(-1.,-8.,0.));
#1710=CARTESIAN_POINT('Ctrl Pts',(-1.,-8.,5.91607978309962));
#1711=CARTESIAN_POINT('Ctrl Pts',(-1.,-7.87418345801814,5.91607978309962));
#1712=CARTESIAN_POINT('Ctrl Pts',(-0.974807371025508,-7.74014451903107,
5.92050853647266));
#1713=CARTESIAN_POINT('Ctrl Pts',(-0.872681546203438,-7.49383674704903,
5.93642128117897));
#1714=CARTESIAN_POINT('Ctrl Pts',(-0.795760896484534,-7.38154733411144,
5.94766633611059));
#1715=CARTESIAN_POINT('Ctrl Pts',(-0.61845503374177,-7.20424147136868,5.96870867068992));
#1716=CARTESIAN_POINT('Ctrl Pts',(-0.506164604242066,-7.12731896437637,
5.97988517961729));
#1717=CARTESIAN_POINT('Ctrl Pts',(-0.25985334006496,-7.0251917910001,5.99564055034545));
#1718=CARTESIAN_POINT('Ctrl Pts',(-0.125813181561402,-7.,6.));
#1719=CARTESIAN_POINT('Ctrl Pts',(0.125813181561403,-7.,6.));
#1720=CARTESIAN_POINT('Ctrl Pts',(0.259853340064961,-7.0251917910001,5.99564055034545));
#1721=CARTESIAN_POINT('Ctrl Pts',(0.506164604242067,-7.12731896437637,5.97988517961729));
#1722=CARTESIAN_POINT('Ctrl Pts',(0.618455033741771,-7.20424147136868,5.96870867068992));
#1723=CARTESIAN_POINT('Ctrl Pts',(0.795760896484535,-7.38154733411144,5.94766633611059));
#1724=CARTESIAN_POINT('Ctrl Pts',(0.872681546203439,-7.49383674704903,5.93642128117897));
#1725=CARTESIAN_POINT('Ctrl Pts',(0.974807371025509,-7.74014451903108,5.92050853647266));
#1726=CARTESIAN_POINT('Ctrl Pts',(1.,-7.87418345801814,5.91607978309962));
#1727=CARTESIAN_POINT('Ctrl Pts',(1.,-8.12581654198186,5.91607978309962));
#1728=CARTESIAN_POINT('Ctrl Pts',(0.974807371025508,-8.25985548096893,5.92050853647266));
#1729=CARTESIAN_POINT('Ctrl Pts',(0.872681546203439,-8.50616325295097,5.93642128117897));
#1730=CARTESIAN_POINT('Ctrl Pts',(0.795760896484535,-8.61845266588856,5.94766633611059));
#1731=CARTESIAN_POINT('Ctrl Pts',(0.618455033741771,-8.79575852863132,5.96870867068992));
#1732=CARTESIAN_POINT('Ctrl Pts',(0.506164604242067,-8.87268103562363,5.97988517961729));
#1733=CARTESIAN_POINT('Ctrl Pts',(0.25985334006496,-8.97480820899991,5.99564055034545));
#1734=CARTESIAN_POINT('Ctrl Pts',(0.125813181561403,-9.,6.));
#1735=CARTESIAN_POINT('Ctrl Pts',(-0.125813181561403,-9.,6.));
#1736=CARTESIAN_POINT('Ctrl Pts',(-0.25985334006496,-8.97480820899991,5.99564055034545));
#1737=CARTESIAN_POINT('Ctrl Pts',(-0.506164604242066,-8.87268103562363,
5.97988517961729));
#1738=CARTESIAN_POINT('Ctrl Pts',(-0.618455033741771,-8.79575852863132,
5.96870867068992));
#1739=CARTESIAN_POINT('Ctrl Pts',(-0.795760896484535,-8.61845266588856,
5.94766633611059));
#1740=CARTESIAN_POINT('Ctrl Pts',(-0.872681546203439,-8.50616325295097,
5.93642128117897));
#1741=CARTESIAN_POINT('Ctrl Pts',(-0.974807371025509,-8.25985548096893,
5.92050853647266));
#1742=CARTESIAN_POINT('Ctrl Pts',(-1.,-8.12581654198186,5.91607978309962));
#1743=CARTESIAN_POINT('Ctrl Pts',(-1.,-8.,5.91607978309962));
#1744=CARTESIAN_POINT('Origin',(1.25,-6.,3.29967103839267));
#1745=CARTESIAN_POINT('',(1.25,-10.,4.84122918275927));
#1746=CARTESIAN_POINT('',(1.25,-10.,3.79967103839267));
#1747=CARTESIAN_POINT('',(1.25,-10.,1.64983551919633));
#1748=CARTESIAN_POINT('',(1.25,-6.,4.84122918275927));
#1749=CARTESIAN_POINT('',(1.25,-6.,4.84122918275927));
#1750=CARTESIAN_POINT('',(1.25,-6.,3.79967103839267));
#1751=CARTESIAN_POINT('',(1.25,-6.,6.32461990770089));
#1752=CARTESIAN_POINT('',(1.25,-6.,3.79967103839267));
#1753=CARTESIAN_POINT('Origin',(1.25,-6.,4.84122918275927));
#1754=CARTESIAN_POINT('',(-1.25,-10.,4.84122918275927));
#1755=CARTESIAN_POINT('',(0.625,-10.,4.84122918275927));
#1756=CARTESIAN_POINT('',(-1.25,-6.,4.84122918275927));
#1757=CARTESIAN_POINT('',(-1.25,-6.,4.84122918275927));
#1758=CARTESIAN_POINT('',(-1.25,-6.,4.84122918275927));
#1759=CARTESIAN_POINT('Origin',(-1.25,-6.,4.84122918275927));
#1760=CARTESIAN_POINT('',(-1.25,-10.,3.79967103839267));
#1761=CARTESIAN_POINT('',(-1.25,-10.,2.42061459137964));
#1762=CARTESIAN_POINT('',(-1.25,-6.,3.79967103839267));
#1763=CARTESIAN_POINT('',(-1.25,-6.,3.79967103839267));
#1764=CARTESIAN_POINT('',(-1.25,-6.,3.79967103839267));
#1765=CARTESIAN_POINT('Origin',(0.,-6.,0.));
#1766=CARTESIAN_POINT('Origin',(0.,-6.,0.));
#1767=CARTESIAN_POINT('Origin',(0.,-6.,0.));
#1768=CARTESIAN_POINT('Origin',(0.,-10.,0.));
#1769=CARTESIAN_POINT('Origin',(-1.5,0.,12.4096736459909));
#1770=CARTESIAN_POINT('',(-1.5,0.,12.4096736459909));
#1771=CARTESIAN_POINT('',(-1.5,0.,-12.4096736459909));
#1772=CARTESIAN_POINT('',(-1.5,0.,6.20483682299543));
#1773=CARTESIAN_POINT('',(-1.5,-2.5,12.4096736459909));
#1774=CARTESIAN_POINT('',(-1.5,0.,12.4096736459909));
#1775=CARTESIAN_POINT('',(-1.5,-2.5,-12.4096736459909));
#1776=CARTESIAN_POINT('',(-1.5,-2.5,15.2595947063511));
#1777=CARTESIAN_POINT('',(-1.5,0.,-12.4096736459909));
#1778=CARTESIAN_POINT('Origin',(1.5,0.,-12.4096736459909));
#1779=CARTESIAN_POINT('',(1.5,0.,-12.4096736459909));
#1780=CARTESIAN_POINT('',(1.5,0.,12.4096736459909));
#1781=CARTESIAN_POINT('',(1.5,0.,-6.20483682299543));
#1782=CARTESIAN_POINT('',(1.5,-2.5,-12.4096736459909));
#1783=CARTESIAN_POINT('',(1.5,0.,-12.4096736459909));
#1784=CARTESIAN_POINT('',(1.5,-2.5,12.4096736459909));
#1785=CARTESIAN_POINT('',(1.5,-2.5,-15.2595947063511));
#1786=CARTESIAN_POINT('',(1.5,0.,12.4096736459909));
#1787=CARTESIAN_POINT('Origin',(2.77555756156289E-16,-2.5,0.));
#1788=CARTESIAN_POINT('Origin',(0.,-2.5,0.));
#1789=CARTESIAN_POINT('Origin',(0.,-2.5,0.));
#1790=CARTESIAN_POINT('Origin',(0.,0.,0.));
#1791=CARTESIAN_POINT('Origin',(0.,0.,0.));
#1792=CARTESIAN_POINT('Origin',(0.,0.,0.));
#1793=CARTESIAN_POINT('',(-12.5,0.,-1.53080849893419E-15));
#1794=CARTESIAN_POINT('Origin',(0.,0.,0.));
#1795=CARTESIAN_POINT('Origin',(0.,0.,0.));
#1796=CARTESIAN_POINT('Origin',(0.,-6.,0.));
#1797=CARTESIAN_POINT('',(-6.,-10.,-7.34788079488412E-16));
#1798=CARTESIAN_POINT('Origin',(0.,-10.,0.));
#1799=CARTESIAN_POINT('',(-6.,-6.,-7.34788079488412E-16));
#1800=CARTESIAN_POINT('',(-6.,-6.,-7.34788079488412E-16));
#1801=CARTESIAN_POINT('Origin',(0.,-6.,0.));
#1802=CARTESIAN_POINT('Origin',(0.,-10.,0.));
#1803=CARTESIAN_POINT('Origin',(0.,-6.,0.));
#1804=CARTESIAN_POINT('',(-12.5,-6.,1.53080849893419E-15));
#1805=CARTESIAN_POINT('Origin',(0.,-6.,0.));
#1806=CARTESIAN_POINT('Origin',(0.,0.,0.));
#1807=CARTESIAN_POINT('',(-12.5,0.,-1.53080849893419E-15));
#1808=CARTESIAN_POINT('',(0.,0.,0.));
#1809=CARTESIAN_POINT('Origin',(12.4096736459909,4.,0.499999999999999));
#1810=CARTESIAN_POINT('',(-12.4096736459909,4.,0.499999999999999));
#1811=CARTESIAN_POINT('',(12.4096736459909,4.,0.499999999999999));
#1812=CARTESIAN_POINT('',(6.20483682299543,4.,0.499999999999999));
#1813=CARTESIAN_POINT('',(-12.4096736459909,6.5,0.499999999999999));
#1814=CARTESIAN_POINT('',(-12.4096736459909,4.,0.499999999999999));
#1815=CARTESIAN_POINT('',(12.4096736459909,6.5,0.499999999999999));
#1816=CARTESIAN_POINT('',(-18.9791024697249,6.5,0.499999999999999));
#1817=CARTESIAN_POINT('',(12.4096736459909,4.,0.499999999999999));
#1818=CARTESIAN_POINT('Origin',(-12.4096736459909,4.,3.5));
#1819=CARTESIAN_POINT('',(12.4096736459909,4.,3.5));
#1820=CARTESIAN_POINT('',(-12.4096736459909,4.,3.5));
#1821=CARTESIAN_POINT('',(-6.20483682299543,4.,3.5));
#1822=CARTESIAN_POINT('',(12.4096736459909,6.5,3.5));
#1823=CARTESIAN_POINT('',(12.4096736459909,4.,3.5));
#1824=CARTESIAN_POINT('',(-12.4096736459909,6.5,3.5));
#1825=CARTESIAN_POINT('',(18.9791024697249,6.5,3.5));
#1826=CARTESIAN_POINT('',(-12.4096736459909,4.,3.5));
#1827=CARTESIAN_POINT('Origin',(0.,6.5,2.));
#1828=CARTESIAN_POINT('Origin',(0.,6.5,2.));
#1829=CARTESIAN_POINT('',(12.5,6.5,2.));
#1830=CARTESIAN_POINT('Origin',(0.,6.5,2.));
#1831=CARTESIAN_POINT('Origin',(0.,6.5,2.));
#1832=CARTESIAN_POINT('Origin',(0.,4.,2.));
#1833=CARTESIAN_POINT('Origin',(0.,4.,2.));
#1834=CARTESIAN_POINT('Origin',(0.,4.,2.));
#1835=CARTESIAN_POINT('Origin',(0.,4.,2.));
#1836=CARTESIAN_POINT('Origin',(-1.5,0.,14.4096736459909));
#1837=CARTESIAN_POINT('',(-1.5,0.,-10.4096736459909));
#1838=CARTESIAN_POINT('',(-1.5,0.,14.4096736459909));
#1839=CARTESIAN_POINT('',(-1.5,0.,8.20483682299543));
#1840=CARTESIAN_POINT('',(-1.5,-2.5,-10.4096736459909));
#1841=CARTESIAN_POINT('',(-1.5,0.,-10.4096736459909));
#1842=CARTESIAN_POINT('',(-1.5,-2.5,14.4096736459909));
#1843=CARTESIAN_POINT('',(-1.5,-2.5,17.2595947063511));
#1844=CARTESIAN_POINT('',(-1.5,0.,14.4096736459909));
#1845=CARTESIAN_POINT('Origin',(1.5,0.,-10.4096736459909));
#1846=CARTESIAN_POINT('',(1.5,0.,14.4096736459909));
#1847=CARTESIAN_POINT('',(1.5,0.,-10.4096736459909));
#1848=CARTESIAN_POINT('',(1.5,0.,-4.20483682299543));
#1849=CARTESIAN_POINT('',(1.5,-2.5,14.4096736459909));
#1850=CARTESIAN_POINT('',(1.5,0.,14.4096736459909));
#1851=CARTESIAN_POINT('',(1.5,-2.5,-10.4096736459909));
#1852=CARTESIAN_POINT('',(1.5,-2.5,-13.2595947063511));
#1853=CARTESIAN_POINT('',(1.5,0.,-10.4096736459909));
#1854=CARTESIAN_POINT('Origin',(2.77555756156289E-16,-2.5,2.));
#1855=CARTESIAN_POINT('Origin',(0.,-2.5,2.));
#1856=CARTESIAN_POINT('Origin',(0.,-2.5,2.));
#1857=CARTESIAN_POINT('Origin',(0.,0.,2.));
#1858=CARTESIAN_POINT('Origin',(0.,0.,2.));
#1859=CARTESIAN_POINT('Origin',(0.,0.,2.));
#1860=CARTESIAN_POINT('',(12.5,0.,2.));
#1861=CARTESIAN_POINT('Origin',(0.,0.,2.));
#1862=CARTESIAN_POINT('Origin',(0.,0.,2.));
#1863=CARTESIAN_POINT('Origin',(0.,0.,2.));
#1864=CARTESIAN_POINT('',(12.5,0.,2.));
#1865=CARTESIAN_POINT('',(0.,0.,0.));
#1866=CARTESIAN_POINT('Origin',(2.,12.,2.));
#1867=CARTESIAN_POINT('',(1.,12.,6.84122918275927));
#1868=CARTESIAN_POINT('Origin',(2.,12.,6.84122918275927));
#1869=CARTESIAN_POINT('',(1.,12.,7.91607978309962));
#1870=CARTESIAN_POINT('',(1.,12.,2.));
#1871=CARTESIAN_POINT('',(3.,12.,7.91607978309962));
#1872=CARTESIAN_POINT('Ctrl Pts',(3.,12.,7.91607978309962));
#1873=CARTESIAN_POINT('Ctrl Pts',(3.,11.8741834580181,7.91607978309962));
#1874=CARTESIAN_POINT('Ctrl Pts',(2.97480737102551,11.7401445190311,7.92050853647266));
#1875=CARTESIAN_POINT('Ctrl Pts',(2.87268154620344,11.493836747049,7.93642128117897));
#1876=CARTESIAN_POINT('Ctrl Pts',(2.79576089648453,11.3815473341114,7.94766633611059));
#1877=CARTESIAN_POINT('Ctrl Pts',(2.61845503374177,11.2042414713687,7.96870867068992));
#1878=CARTESIAN_POINT('Ctrl Pts',(2.50616460424207,11.1273189643764,7.97988517961729));
#1879=CARTESIAN_POINT('Ctrl Pts',(2.25985334006496,11.0251917910001,7.99564055034545));
#1880=CARTESIAN_POINT('Ctrl Pts',(2.1258131815614,11.,8.));
#1881=CARTESIAN_POINT('Ctrl Pts',(1.8741868184386,11.,8.));
#1882=CARTESIAN_POINT('Ctrl Pts',(1.74014665993504,11.0251917910001,7.99564055034545));
#1883=CARTESIAN_POINT('Ctrl Pts',(1.49383539575793,11.1273189643764,7.97988517961729));
#1884=CARTESIAN_POINT('Ctrl Pts',(1.38154496625823,11.2042414713687,7.96870867068992));
#1885=CARTESIAN_POINT('Ctrl Pts',(1.20423910351547,11.3815473341114,7.94766633611059));
#1886=CARTESIAN_POINT('Ctrl Pts',(1.12731845379656,11.493836747049,7.93642128117897));
#1887=CARTESIAN_POINT('Ctrl Pts',(1.02519262897449,11.7401445190311,7.92050853647266));
#1888=CARTESIAN_POINT('Ctrl Pts',(1.,11.8741834580181,7.91607978309962));
#1889=CARTESIAN_POINT('Ctrl Pts',(1.,12.,7.91607978309962));
#1890=CARTESIAN_POINT('Ctrl Pts',(1.,12.,7.91607978309962));
#1891=CARTESIAN_POINT('Ctrl Pts',(1.,12.1258165419819,7.91607978309962));
#1892=CARTESIAN_POINT('Ctrl Pts',(1.02519262897449,12.2598554809689,7.92050853647266));
#1893=CARTESIAN_POINT('Ctrl Pts',(1.12731845379656,12.506163252951,7.93642128117897));
#1894=CARTESIAN_POINT('Ctrl Pts',(1.20423910351547,12.6184526658886,7.94766633611059));
#1895=CARTESIAN_POINT('Ctrl Pts',(1.38154496625823,12.7957585286313,7.96870867068992));
#1896=CARTESIAN_POINT('Ctrl Pts',(1.49383539575793,12.8726810356236,7.97988517961729));
#1897=CARTESIAN_POINT('Ctrl Pts',(1.74014665993504,12.9748082089999,7.99564055034545));
#1898=CARTESIAN_POINT('Ctrl Pts',(1.8741868184386,13.,8.));
#1899=CARTESIAN_POINT('Ctrl Pts',(2.1258131815614,13.,8.));
#1900=CARTESIAN_POINT('Ctrl Pts',(2.25985334006496,12.9748082089999,7.99564055034545));
#1901=CARTESIAN_POINT('Ctrl Pts',(2.50616460424207,12.8726810356236,7.97988517961729));
#1902=CARTESIAN_POINT('Ctrl Pts',(2.61845503374177,12.7957585286313,7.96870867068992));
#1903=CARTESIAN_POINT('Ctrl Pts',(2.79576089648453,12.6184526658886,7.94766633611059));
#1904=CARTESIAN_POINT('Ctrl Pts',(2.87268154620344,12.506163252951,7.93642128117897));
#1905=CARTESIAN_POINT('Ctrl Pts',(2.97480737102551,12.2598554809689,7.92050853647266));
#1906=CARTESIAN_POINT('Ctrl Pts',(3.,12.1258165419819,7.91607978309962));
#1907=CARTESIAN_POINT('Ctrl Pts',(3.,12.,7.91607978309962));
#1908=CARTESIAN_POINT('Origin',(3.25,10.,6.84122918275927));
#1909=CARTESIAN_POINT('',(3.25,14.,6.84122918275927));
#1910=CARTESIAN_POINT('',(0.75,14.,6.84122918275927));
#1911=CARTESIAN_POINT('',(2.625,14.,6.84122918275927));
#1912=CARTESIAN_POINT('',(3.25,10.,6.84122918275927));
#1913=CARTESIAN_POINT('',(3.25,10.,6.84122918275927));
#1914=CARTESIAN_POINT('',(0.75,10.,6.84122918275927));
#1915=CARTESIAN_POINT('',(0.75,10.,6.84122918275927));
#1916=CARTESIAN_POINT('',(0.75,10.,6.84122918275927));
#1917=CARTESIAN_POINT('Origin',(0.75,10.,6.84122918275927));
#1918=CARTESIAN_POINT('',(0.75,14.,5.79967103839267));
#1919=CARTESIAN_POINT('',(0.75,14.,4.42061459137964));
#1920=CARTESIAN_POINT('',(0.75,10.,5.79967103839267));
#1921=CARTESIAN_POINT('',(0.75,10.,5.79967103839267));
#1922=CARTESIAN_POINT('',(0.75,10.,5.79967103839267));
#1923=CARTESIAN_POINT('Origin',(3.25,10.,5.29967103839267));
#1924=CARTESIAN_POINT('',(3.25,14.,5.79967103839267));
#1925=CARTESIAN_POINT('',(3.25,14.,3.64983551919633));
#1926=CARTESIAN_POINT('',(3.25,10.,5.79967103839267));
#1927=CARTESIAN_POINT('',(3.25,10.,5.79967103839267));
#1928=CARTESIAN_POINT('',(3.25,10.,8.32461990770089));
#1929=CARTESIAN_POINT('Origin',(2.,14.,2.));
#1930=CARTESIAN_POINT('',(8.,14.,2.));
#1931=CARTESIAN_POINT('Origin',(2.,14.,2.));
#1932=CARTESIAN_POINT('Origin',(2.,14.,2.));
#1933=CARTESIAN_POINT('Origin',(2.,10.,2.));
#1934=CARTESIAN_POINT('Origin',(2.,10.,2.));
#1935=CARTESIAN_POINT('Origin',(2.,10.,2.));
#1936=CARTESIAN_POINT('',(8.,10.,2.));
#1937=CARTESIAN_POINT('',(8.,10.,2.));
#1938=CARTESIAN_POINT('Origin',(2.,10.,2.));
#1939=CARTESIAN_POINT('Origin',(2.,10.,2.));
#1940=CARTESIAN_POINT('',(14.5,10.,2.));
#1941=CARTESIAN_POINT('Origin',(2.,10.,2.));
#1942=CARTESIAN_POINT('Origin',(14.4096736459909,4.,0.499999999999999));
#1943=CARTESIAN_POINT('',(14.4096736459909,4.,0.499999999999999));
#1944=CARTESIAN_POINT('',(-10.4096736459909,4.,0.499999999999999));
#1945=CARTESIAN_POINT('',(8.20483682299543,4.,0.499999999999999));
#1946=CARTESIAN_POINT('',(14.4096736459909,6.5,0.499999999999999));
#1947=CARTESIAN_POINT('',(14.4096736459909,4.,0.499999999999999));
#1948=CARTESIAN_POINT('',(-10.4096736459909,6.5,0.499999999999999));
#1949=CARTESIAN_POINT('',(-16.9791024697249,6.5,0.499999999999999));
#1950=CARTESIAN_POINT('',(-10.4096736459909,4.,0.499999999999999));
#1951=CARTESIAN_POINT('Origin',(-10.4096736459909,4.,3.5));
#1952=CARTESIAN_POINT('',(-10.4096736459909,4.,3.5));
#1953=CARTESIAN_POINT('',(14.4096736459909,4.,3.5));
#1954=CARTESIAN_POINT('',(-4.20483682299543,4.,3.5));
#1955=CARTESIAN_POINT('',(-10.4096736459909,6.5,3.5));
#1956=CARTESIAN_POINT('',(-10.4096736459909,4.,3.5));
#1957=CARTESIAN_POINT('',(14.4096736459909,6.5,3.5));
#1958=CARTESIAN_POINT('',(20.9791024697249,6.5,3.5));
#1959=CARTESIAN_POINT('',(14.4096736459909,4.,3.5));
#1960=CARTESIAN_POINT('Origin',(2.,6.5,2.));
#1961=CARTESIAN_POINT('Origin',(2.,6.5,2.));
#1962=CARTESIAN_POINT('',(14.5,6.5,2.));
#1963=CARTESIAN_POINT('Origin',(2.,6.5,2.));
#1964=CARTESIAN_POINT('Origin',(2.,6.5,2.));
#1965=CARTESIAN_POINT('Origin',(2.,4.,2.));
#1966=CARTESIAN_POINT('Origin',(2.,4.,2.));
#1967=CARTESIAN_POINT('Origin',(2.,4.,2.));
#1968=CARTESIAN_POINT('Origin',(2.,4.,2.));
#1969=CARTESIAN_POINT('Origin',(2.,4.,2.));
#1970=CARTESIAN_POINT('',(14.5,4.,2.));
#1971=CARTESIAN_POINT('Origin',(2.,10.,2.));
#1972=CARTESIAN_POINT('',(0.,0.,0.));
#1973=CARTESIAN_POINT('Origin',(3.25,10.,5.29967103839267));
#1974=CARTESIAN_POINT('',(3.25,16.,5.79967103839267));
#1975=CARTESIAN_POINT('',(3.25,10.,5.79967103839267));
#1976=CARTESIAN_POINT('',(3.25,10.,5.79967103839267));
#1977=CARTESIAN_POINT('',(3.25,16.,5.29967103839267));
#1978=CARTESIAN_POINT('',(3.25,16.,8.32461990770089));
#1979=CARTESIAN_POINT('',(3.25,10.,5.29967103839267));
#1980=CARTESIAN_POINT('',(3.25,10.,5.29967103839267));
#1981=CARTESIAN_POINT('',(3.25,10.,3.64983551919633));
#1982=CARTESIAN_POINT('Origin',(0.75,10.,5.29967103839267));
#1983=CARTESIAN_POINT('',(0.75,10.,5.29967103839267));
#1984=CARTESIAN_POINT('',(1.375,10.,5.29967103839267));
#1985=CARTESIAN_POINT('',(0.75,16.,5.29967103839267));
#1986=CARTESIAN_POINT('',(0.75,16.,5.29967103839267));
#1987=CARTESIAN_POINT('',(0.75,10.,5.29967103839267));
#1988=CARTESIAN_POINT('Origin',(0.75,10.,6.84122918275927));
#1989=CARTESIAN_POINT('',(0.75,10.,5.79967103839267));
#1990=CARTESIAN_POINT('',(0.75,16.,5.79967103839267));
#1991=CARTESIAN_POINT('',(0.75,10.,5.79967103839267));
#1992=CARTESIAN_POINT('',(0.75,10.,4.42061459137964));
#1993=CARTESIAN_POINT('',(0.75,16.,5.79967103839267));
#1994=CARTESIAN_POINT('Origin',(2.,16.,6.07045011057597));
#1995=CARTESIAN_POINT('Origin',(2.,16.,2.));
#1996=CARTESIAN_POINT('Origin',(2.,10.,2.));
#1997=CARTESIAN_POINT('',(-2.,10.,2.));
#1998=CARTESIAN_POINT('Origin',(2.,10.,2.));
#1999=CARTESIAN_POINT('Origin',(2.,10.,2.));
#2000=CARTESIAN_POINT('Origin',(2.,10.,2.));
#2001=CARTESIAN_POINT('',(-2.,34.,2.));
#2002=CARTESIAN_POINT('',(-2.,10.,2.));
#2003=CARTESIAN_POINT('Origin',(2.,34.,2.));
#2004=CARTESIAN_POINT('Origin',(2.,34.,2.));
#2005=CARTESIAN_POINT('',(0.,0.,0.));
#2006=CARTESIAN_POINT('Origin',(3.25,10.,6.84122918275927));
#2007=CARTESIAN_POINT('',(0.75,10.,6.84122918275927));
#2008=CARTESIAN_POINT('',(3.25,10.,6.84122918275927));
#2009=CARTESIAN_POINT('',(0.75,10.,6.84122918275927));
#2010=CARTESIAN_POINT('',(3.25,16.,6.84122918275927));
#2011=CARTESIAN_POINT('',(3.25,10.,6.84122918275927));
#2012=CARTESIAN_POINT('',(0.75,16.,6.84122918275927));
#2013=CARTESIAN_POINT('',(0.75,16.,6.84122918275927));
#2014=CARTESIAN_POINT('',(0.75,10.,6.84122918275927));
#2015=CARTESIAN_POINT('Origin',(3.25,10.,5.29967103839267));
#2016=CARTESIAN_POINT('',(3.25,10.,5.29967103839267));
#2017=CARTESIAN_POINT('',(3.25,10.,8.32461990770089));
#2018=CARTESIAN_POINT('',(3.25,16.,5.29967103839267));
#2019=CARTESIAN_POINT('',(3.25,10.,5.29967103839267));
#2020=CARTESIAN_POINT('',(3.25,16.,8.32461990770089));
#2021=CARTESIAN_POINT('Origin',(0.75,10.,5.29967103839267));
#2022=CARTESIAN_POINT('',(0.75,10.,5.29967103839267));
#2023=CARTESIAN_POINT('',(0.75,10.,5.29967103839267));
#2024=CARTESIAN_POINT('',(0.75,16.,5.29967103839267));
#2025=CARTESIAN_POINT('',(0.75,10.,5.29967103839267));
#2026=CARTESIAN_POINT('',(0.75,16.,5.29967103839267));
#2027=CARTESIAN_POINT('Origin',(0.75,10.,6.84122918275927));
#2028=CARTESIAN_POINT('',(0.75,10.,5.79967103839267));
#2029=CARTESIAN_POINT('',(0.75,16.,5.79967103839267));
#2030=CARTESIAN_POINT('Origin',(2.,16.,6.07045011057597));
#2031=CARTESIAN_POINT('Origin',(2.,10.,6.07045011057597));
#2032=CARTESIAN_POINT('',(0.,0.,0.));
#2033=CARTESIAN_POINT('Origin',(1.25,-6.,3.29967103839267));
#2034=CARTESIAN_POINT('',(1.25,-6.,3.79967103839267));
#2035=CARTESIAN_POINT('',(1.25,-12.,3.79967103839267));
#2036=CARTESIAN_POINT('',(1.25,-6.,3.79967103839267));
#2037=CARTESIAN_POINT('',(1.25,-6.,3.29967103839267));
#2038=CARTESIAN_POINT('',(1.25,-6.,1.64983551919633));
#2039=CARTESIAN_POINT('',(1.25,-12.,3.29967103839267));
#2040=CARTESIAN_POINT('',(1.25,-6.,3.29967103839267));
#2041=CARTESIAN_POINT('',(1.25,-12.,6.32461990770089));
#2042=CARTESIAN_POINT('Origin',(0.,-12.,4.07045011057597));
#2043=CARTESIAN_POINT('',(-1.25,-12.,3.79967103839267));
#2044=CARTESIAN_POINT('Origin',(0.,-12.,0.));
#2045=CARTESIAN_POINT('',(-1.25,-12.,3.29967103839267));
#2046=CARTESIAN_POINT('',(-1.25,-12.,3.29967103839267));
#2047=CARTESIAN_POINT('',(-1.25,-12.,3.79967103839267));
#2048=CARTESIAN_POINT('Origin',(-1.25,-6.,3.29967103839267));
#2049=CARTESIAN_POINT('',(-1.25,-6.,3.29967103839267));
#2050=CARTESIAN_POINT('',(-0.625,-6.,3.29967103839267));
#2051=CARTESIAN_POINT('',(-1.25,-6.,3.29967103839267));
#2052=CARTESIAN_POINT('Origin',(-1.25,-6.,4.84122918275927));
#2053=CARTESIAN_POINT('',(-1.25,-6.,3.79967103839267));
#2054=CARTESIAN_POINT('',(-1.25,-6.,3.79967103839267));
#2055=CARTESIAN_POINT('',(-1.25,-6.,2.42061459137964));
#2056=CARTESIAN_POINT('Origin',(0.,-6.,0.));
#2057=CARTESIAN_POINT('',(-4.,-30.,-4.89858719658941E-16));
#2058=CARTESIAN_POINT('Origin',(0.,-30.,0.));
#2059=CARTESIAN_POINT('',(-4.,-6.,-4.89858719658941E-16));
#2060=CARTESIAN_POINT('',(-4.,-6.,-4.89858719658941E-16));
#2061=CARTESIAN_POINT('Origin',(0.,-6.,0.));
#2062=CARTESIAN_POINT('Origin',(0.,-6.,0.));
#2063=CARTESIAN_POINT('Origin',(0.,-30.,0.));
#2064=CARTESIAN_POINT('Origin',(0.,-6.,0.));
#2065=CARTESIAN_POINT('',(0.,0.,0.));
#2066=CARTESIAN_POINT('Origin',(1.25,-6.,4.84122918275927));
#2067=CARTESIAN_POINT('',(-1.25,-6.,4.84122918275927));
#2068=CARTESIAN_POINT('',(1.25,-6.,4.84122918275927));
#2069=CARTESIAN_POINT('',(-1.25,-6.,4.84122918275927));
#2070=CARTESIAN_POINT('',(-1.25,-12.,4.84122918275927));
#2071=CARTESIAN_POINT('',(-1.25,-6.,4.84122918275927));
#2072=CARTESIAN_POINT('',(1.25,-12.,4.84122918275927));
#2073=CARTESIAN_POINT('',(-1.25,-12.,4.84122918275927));
#2074=CARTESIAN_POINT('',(1.25,-6.,4.84122918275927));
#2075=CARTESIAN_POINT('Origin',(1.25,-6.,3.29967103839267));
#2076=CARTESIAN_POINT('',(1.25,-6.,3.29967103839267));
#2077=CARTESIAN_POINT('',(1.25,-6.,6.32461990770089));
#2078=CARTESIAN_POINT('',(1.25,-12.,3.29967103839267));
#2079=CARTESIAN_POINT('',(1.25,-12.,6.32461990770089));
#2080=CARTESIAN_POINT('',(1.25,-6.,3.29967103839267));
#2081=CARTESIAN_POINT('Origin',(-1.25,-6.,3.29967103839267));
#2082=CARTESIAN_POINT('',(-1.25,-6.,3.29967103839267));
#2083=CARTESIAN_POINT('',(-1.25,-6.,3.29967103839267));
#2084=CARTESIAN_POINT('',(-1.25,-12.,3.29967103839267));
#2085=CARTESIAN_POINT('',(-1.25,-12.,3.29967103839267));
#2086=CARTESIAN_POINT('',(-1.25,-6.,3.29967103839267));
#2087=CARTESIAN_POINT('Origin',(-1.25,-6.,4.84122918275927));
#2088=CARTESIAN_POINT('',(-1.25,-6.,3.79967103839267));
#2089=CARTESIAN_POINT('',(-1.25,-12.,3.79967103839267));
#2090=CARTESIAN_POINT('Origin',(0.,-12.,4.07045011057597));
#2091=CARTESIAN_POINT('Origin',(0.,-6.,4.07045011057597));
#2092=CARTESIAN_POINT('',(0.,0.,0.));
#2093=CARTESIAN_POINT('',(0.,0.,-2.));
#2094=CARTESIAN_POINT('',(-2.,0.,-2.));
#2095=CARTESIAN_POINT('',(-2.,0.,-2.));
#2096=CARTESIAN_POINT('',(-2.,0.,-2.));
#2097=CARTESIAN_POINT('',(0.,0.,0.));
#2098=CARTESIAN_POINT('',(0.,0.,0.));
#2099=UNCERTAINTY_MEASURE_WITH_UNIT(LENGTH_MEASURE(0.01),#2117,
'DISTANCE_ACCURACY_VALUE',
'Maximum model space distance between geometric entities at asserted c
onnectivities');
#2100=UNCERTAINTY_MEASURE_WITH_UNIT(LENGTH_MEASURE(0.01),#2117,
'DISTANCE_ACCURACY_VALUE',
'Maximum model space distance between geometric entities at asserted c
onnectivities');
#2101=UNCERTAINTY_MEASURE_WITH_UNIT(LENGTH_MEASURE(0.01),#2117,
'DISTANCE_ACCURACY_VALUE',
'Maximum model space distance between geometric entities at asserted c
onnectivities');
#2102=UNCERTAINTY_MEASURE_WITH_UNIT(LENGTH_MEASURE(0.01),#2117,
'DISTANCE_ACCURACY_VALUE',
'Maximum model space distance between geometric entities at asserted c
onnectivities');
#2103=UNCERTAINTY_MEASURE_WITH_UNIT(LENGTH_MEASURE(0.01),#2117,
'DISTANCE_ACCURACY_VALUE',
'Maximum model space distance between geometric entities at asserted c
onnectivities');
#2104=UNCERTAINTY_MEASURE_WITH_UNIT(LENGTH_MEASURE(0.01),#2117,
'DISTANCE_ACCURACY_VALUE',
'Maximum model space distance between geometric entities at asserted c
onnectivities');
#2105=UNCERTAINTY_MEASURE_WITH_UNIT(LENGTH_MEASURE(0.01),#2117,
'DISTANCE_ACCURACY_VALUE',
'Maximum model space distance between geometric entities at asserted c
onnectivities');
#2106=UNCERTAINTY_MEASURE_WITH_UNIT(LENGTH_MEASURE(0.01),#2117,
'DISTANCE_ACCURACY_VALUE',
'Maximum model space distance between geometric entities at asserted c
onnectivities');
#2107=UNCERTAINTY_MEASURE_WITH_UNIT(LENGTH_MEASURE(0.01),#2117,
'DISTANCE_ACCURACY_VALUE',
'Maximum model space distance between geometric entities at asserted c
onnectivities');
#2108=(
GEOMETRIC_REPRESENTATION_CONTEXT(3)
GLOBAL_UNCERTAINTY_ASSIGNED_CONTEXT((#2099))
GLOBAL_UNIT_ASSIGNED_CONTEXT((#2117,#2119,#2120))
REPRESENTATION_CONTEXT('','3D')
);
#2109=(
GEOMETRIC_REPRESENTATION_CONTEXT(3)
GLOBAL_UNCERTAINTY_ASSIGNED_CONTEXT((#2100))
GLOBAL_UNIT_ASSIGNED_CONTEXT((#2117,#2119,#2120))
REPRESENTATION_CONTEXT('','3D')
);
#2110=(
GEOMETRIC_REPRESENTATION_CONTEXT(3)
GLOBAL_UNCERTAINTY_ASSIGNED_CONTEXT((#2101))
GLOBAL_UNIT_ASSIGNED_CONTEXT((#2117,#2119,#2120))
REPRESENTATION_CONTEXT('','3D')
);
#2111=(
GEOMETRIC_REPRESENTATION_CONTEXT(3)
GLOBAL_UNCERTAINTY_ASSIGNED_CONTEXT((#2102))
GLOBAL_UNIT_ASSIGNED_CONTEXT((#2117,#2119,#2120))
REPRESENTATION_CONTEXT('','3D')
);
#2112=(
GEOMETRIC_REPRESENTATION_CONTEXT(3)
GLOBAL_UNCERTAINTY_ASSIGNED_CONTEXT((#2103))
GLOBAL_UNIT_ASSIGNED_CONTEXT((#2117,#2119,#2120))
REPRESENTATION_CONTEXT('','3D')
);
#2113=(
GEOMETRIC_REPRESENTATION_CONTEXT(3)
GLOBAL_UNCERTAINTY_ASSIGNED_CONTEXT((#2104))
GLOBAL_UNIT_ASSIGNED_CONTEXT((#2117,#2119,#2120))
REPRESENTATION_CONTEXT('','3D')
);
#2114=(
GEOMETRIC_REPRESENTATION_CONTEXT(3)
GLOBAL_UNCERTAINTY_ASSIGNED_CONTEXT((#2105))
GLOBAL_UNIT_ASSIGNED_CONTEXT((#2117,#2119,#2120))
REPRESENTATION_CONTEXT('','3D')
);
#2115=(
GEOMETRIC_REPRESENTATION_CONTEXT(3)
GLOBAL_UNCERTAINTY_ASSIGNED_CONTEXT((#2106))
GLOBAL_UNIT_ASSIGNED_CONTEXT((#2117,#2119,#2120))
REPRESENTATION_CONTEXT('','3D')
);
#2116=(
GEOMETRIC_REPRESENTATION_CONTEXT(3)
GLOBAL_UNCERTAINTY_ASSIGNED_CONTEXT((#2107))
GLOBAL_UNIT_ASSIGNED_CONTEXT((#2117,#2119,#2120))
REPRESENTATION_CONTEXT('','3D')
);
#2117=(
LENGTH_UNIT()
NAMED_UNIT(*)
SI_UNIT(.MILLI.,.METRE.)
);
#2118=(
LENGTH_UNIT()
NAMED_UNIT(*)
SI_UNIT($,.METRE.)
);
#2119=(
NAMED_UNIT(*)
PLANE_ANGLE_UNIT()
SI_UNIT($,.RADIAN.)
);
#2120=(
NAMED_UNIT(*)
SI_UNIT($,.STERADIAN.)
SOLID_ANGLE_UNIT()
);
#2121=SHAPE_DEFINITION_REPRESENTATION(#2129,#2144);
#2122=SHAPE_DEFINITION_REPRESENTATION(#2130,#2145);
#2123=SHAPE_DEFINITION_REPRESENTATION(#2131,#2146);
#2124=SHAPE_DEFINITION_REPRESENTATION(#2132,#2147);
#2125=SHAPE_DEFINITION_REPRESENTATION(#2133,#2148);
#2126=SHAPE_DEFINITION_REPRESENTATION(#2134,#2149);
#2127=SHAPE_DEFINITION_REPRESENTATION(#2135,#2150);
#2128=SHAPE_DEFINITION_REPRESENTATION(#2136,#2151);
#2129=PRODUCT_DEFINITION_SHAPE('',$,#2153);
#2130=PRODUCT_DEFINITION_SHAPE('',$,#2154);
#2131=PRODUCT_DEFINITION_SHAPE('',$,#2155);
#2132=PRODUCT_DEFINITION_SHAPE('',$,#2156);
#2133=PRODUCT_DEFINITION_SHAPE('',$,#2157);
#2134=PRODUCT_DEFINITION_SHAPE('',$,#2158);
#2135=PRODUCT_DEFINITION_SHAPE('',$,#2159);
#2136=PRODUCT_DEFINITION_SHAPE('',$,#2160);
#2137=PRODUCT_DEFINITION_SHAPE($,$,#32);
#2138=PRODUCT_DEFINITION_SHAPE($,$,#33);
#2139=PRODUCT_DEFINITION_SHAPE($,$,#34);
#2140=PRODUCT_DEFINITION_SHAPE($,$,#35);
#2141=PRODUCT_DEFINITION_SHAPE($,$,#36);
#2142=PRODUCT_DEFINITION_SHAPE($,$,#37);
#2143=PRODUCT_DEFINITION_SHAPE($,$,#38);
#2144=SHAPE_REPRESENTATION('',(#1232,#1347,#1348,#1349,#1350,#1351,#1352,
#1353),#2108);
#2145=SHAPE_REPRESENTATION('',(#1233),#2109);
#2146=SHAPE_REPRESENTATION('',(#1260),#2110);
#2147=SHAPE_REPRESENTATION('',(#1282),#2111);
#2148=SHAPE_REPRESENTATION('',(#1309),#2112);
#2149=SHAPE_REPRESENTATION('',(#1321),#2113);
#2150=SHAPE_REPRESENTATION('',(#1328),#2114);
#2151=SHAPE_REPRESENTATION('',(#1340),#2115);
#2152=PRODUCT_DEFINITION_CONTEXT('part definition',#2178,'design');
#2153=PRODUCT_DEFINITION('BR-256','BR-256',#2161,#2152);
#2154=PRODUCT_DEFINITION('Hub_01','Hub_01',#2162,#2152);
#2155=PRODUCT_DEFINITION('Middle_Hub','Middle_Hub',#2163,#2152);
#2156=PRODUCT_DEFINITION('Hub_02','Hub_02',#2164,#2152);
#2157=PRODUCT_DEFINITION('Shaft_02','Shaft_02',#2165,#2152);
#2158=PRODUCT_DEFINITION('Pin_02','Pin_02',#2166,#2152);
#2159=PRODUCT_DEFINITION('Shaft_01','Shaft_01',#2167,#2152);
#2160=PRODUCT_DEFINITION('Pin_01','Pin_01',#2168,#2152);
#2161=PRODUCT_DEFINITION_FORMATION('',$,#2180);
#2162=PRODUCT_DEFINITION_FORMATION('',$,#2181);
#2163=PRODUCT_DEFINITION_FORMATION('',$,#2182);
#2164=PRODUCT_DEFINITION_FORMATION('',$,#2183);
#2165=PRODUCT_DEFINITION_FORMATION('',$,#2184);
#2166=PRODUCT_DEFINITION_FORMATION('',$,#2185);
#2167=PRODUCT_DEFINITION_FORMATION('',$,#2186);
#2168=PRODUCT_DEFINITION_FORMATION('',$,#2187);
#2169=PRODUCT_RELATED_PRODUCT_CATEGORY('BR-256','BR-256',(#2180));
#2170=PRODUCT_RELATED_PRODUCT_CATEGORY('Hub_01','Hub_01',(#2181));
#2171=PRODUCT_RELATED_PRODUCT_CATEGORY('Middle_Hub','Middle_Hub',(#2182));
#2172=PRODUCT_RELATED_PRODUCT_CATEGORY('Hub_02','Hub_02',(#2183));
#2173=PRODUCT_RELATED_PRODUCT_CATEGORY('Shaft_02','Shaft_02',(#2184));
#2174=PRODUCT_RELATED_PRODUCT_CATEGORY('Pin_02','Pin_02',(#2185));
#2175=PRODUCT_RELATED_PRODUCT_CATEGORY('Shaft_01','Shaft_01',(#2186));
#2176=PRODUCT_RELATED_PRODUCT_CATEGORY('Pin_01','Pin_01',(#2187));
#2177=APPLICATION_PROTOCOL_DEFINITION('international standard',
'automotive_design',2009,#2178);
#2178=APPLICATION_CONTEXT(
'Core Data for Automotive Mechanical Design Process');
#2179=PRODUCT_CONTEXT('part definition',#2178,'mechanical');
#2180=PRODUCT('BR-256','BR-256',$,(#2179));
#2181=PRODUCT('Hub_01','Hub_01',$,(#2179));
#2182=PRODUCT('Middle_Hub','Middle_Hub',$,(#2179));
#2183=PRODUCT('Hub_02','Hub_02',$,(#2179));
#2184=PRODUCT('Shaft_02','Shaft_02',$,(#2179));
#2185=PRODUCT('Pin_02','Pin_02',$,(#2179));
#2186=PRODUCT('Shaft_01','Shaft_01',$,(#2179));
#2187=PRODUCT('Pin_01','Pin_01',$,(#2179));
#2188=PRESENTATION_STYLE_ASSIGNMENT((#2193));
#2189=PRESENTATION_STYLE_ASSIGNMENT((#2194));
#2190=PRESENTATION_STYLE_ASSIGNMENT((#2195));
#2191=PRESENTATION_STYLE_ASSIGNMENT((#2196));
#2192=PRESENTATION_STYLE_ASSIGNMENT((#2197));
#2193=SURFACE_STYLE_USAGE(.BOTH.,#2198);
#2194=SURFACE_STYLE_USAGE(.BOTH.,#2199);
#2195=SURFACE_STYLE_USAGE(.BOTH.,#2200);
#2196=SURFACE_STYLE_USAGE(.BOTH.,#2201);
#2197=SURFACE_STYLE_USAGE(.BOTH.,#2202);
#2198=SURFACE_SIDE_STYLE('',(#2203));
#2199=SURFACE_SIDE_STYLE('',(#2204));
#2200=SURFACE_SIDE_STYLE('',(#2205));
#2201=SURFACE_SIDE_STYLE('',(#2206));
#2202=SURFACE_SIDE_STYLE('',(#2207));
#2203=SURFACE_STYLE_FILL_AREA(#2208);
#2204=SURFACE_STYLE_FILL_AREA(#2209);
#2205=SURFACE_STYLE_FILL_AREA(#2210);
#2206=SURFACE_STYLE_FILL_AREA(#2211);
#2207=SURFACE_STYLE_FILL_AREA(#2212);
#2208=FILL_AREA_STYLE('Steel - Satin',(#2213));
#2209=FILL_AREA_STYLE('Opaque(0,188,0)',(#2214));
#2210=FILL_AREA_STYLE('Opaque(170,0,255)',(#2215));
#2211=FILL_AREA_STYLE('Opaque(224,224,112)',(#2216));
#2212=FILL_AREA_STYLE('Opaque(235,235,235)',(#2217));
#2213=FILL_AREA_STYLE_COLOUR('Steel - Satin',#2218);
#2214=FILL_AREA_STYLE_COLOUR('Opaque(0,188,0)',#2219);
#2215=FILL_AREA_STYLE_COLOUR('Opaque(170,0,255)',#2220);
#2216=FILL_AREA_STYLE_COLOUR('Opaque(224,224,112)',#2221);
#2217=FILL_AREA_STYLE_COLOUR('Opaque(235,235,235)',#2222);
#2218=COLOUR_RGB('Steel - Satin', 0.09019608, 0.27058824, 0.51372549);
#2219=COLOUR_RGB('Opaque(0,188,0)', 0.09019608, 0.27058824, 0.51372549);
#2220=COLOUR_RGB('Opaque(170,0,255)', 0.66274510, 0.83137255, 0.94901961);
#2221=COLOUR_RGB('Opaque(224,224,112)', 0.31764706, 0.68627451, 0.89019608);
#2222=COLOUR_RGB('Opaque(235,235,235)', 0.40784314, 0.44705882, 0.49803922);
ENDSEC;
END-ISO-10303-21;
